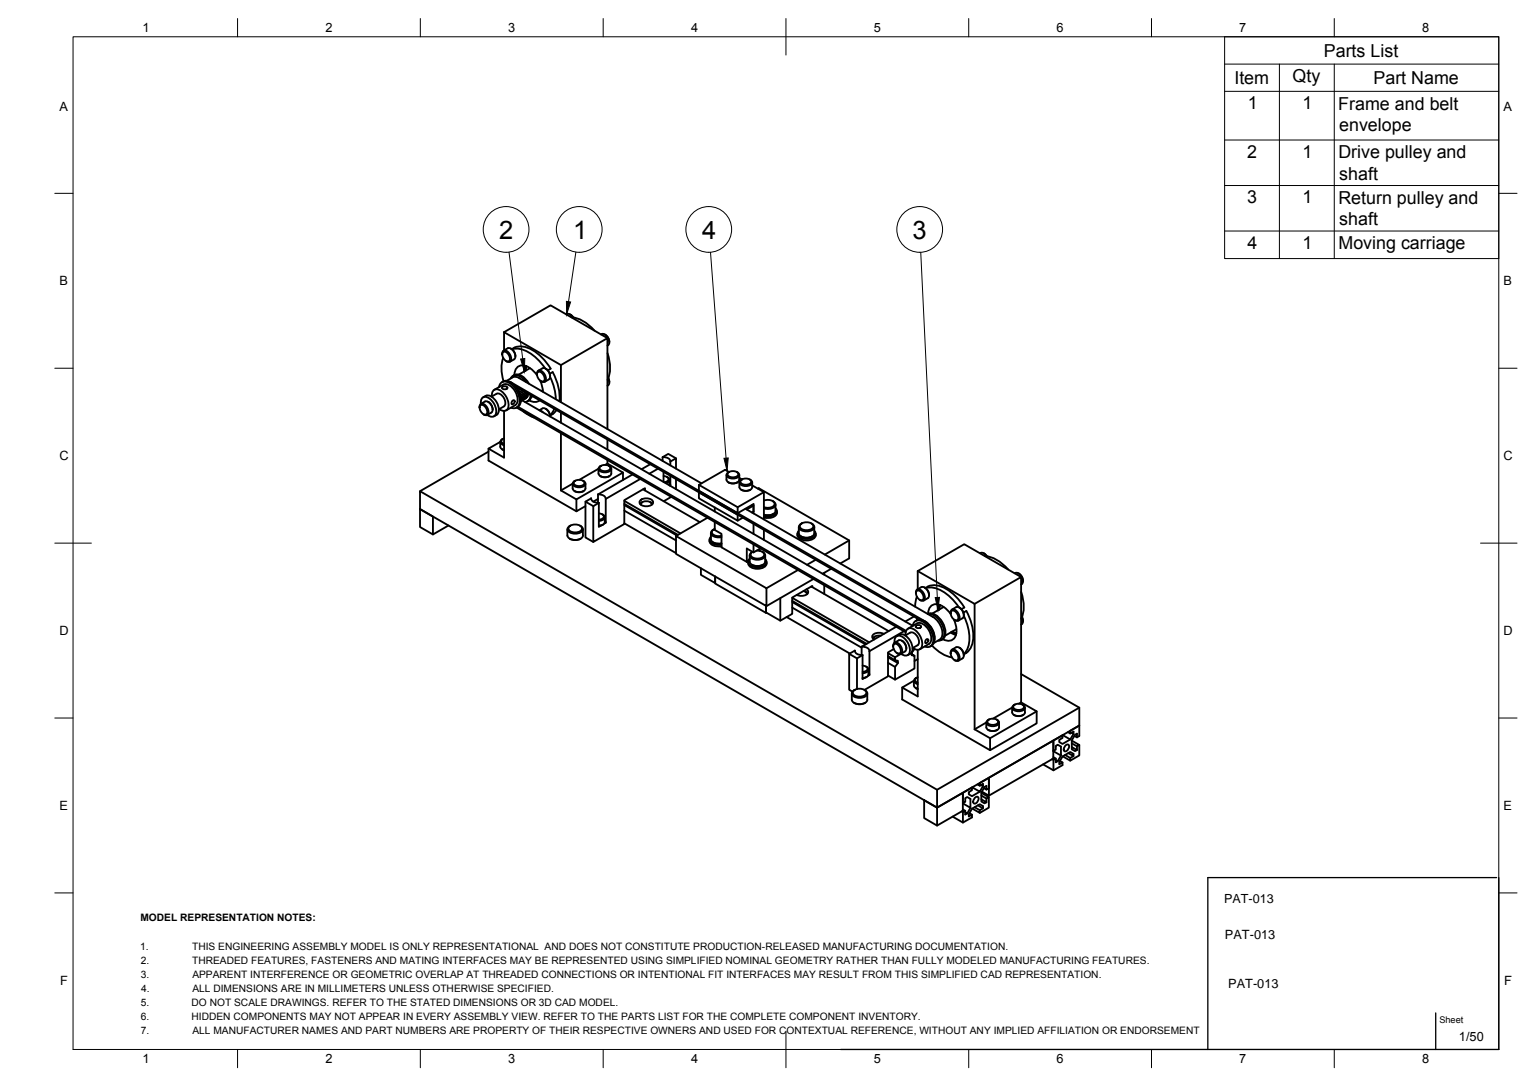
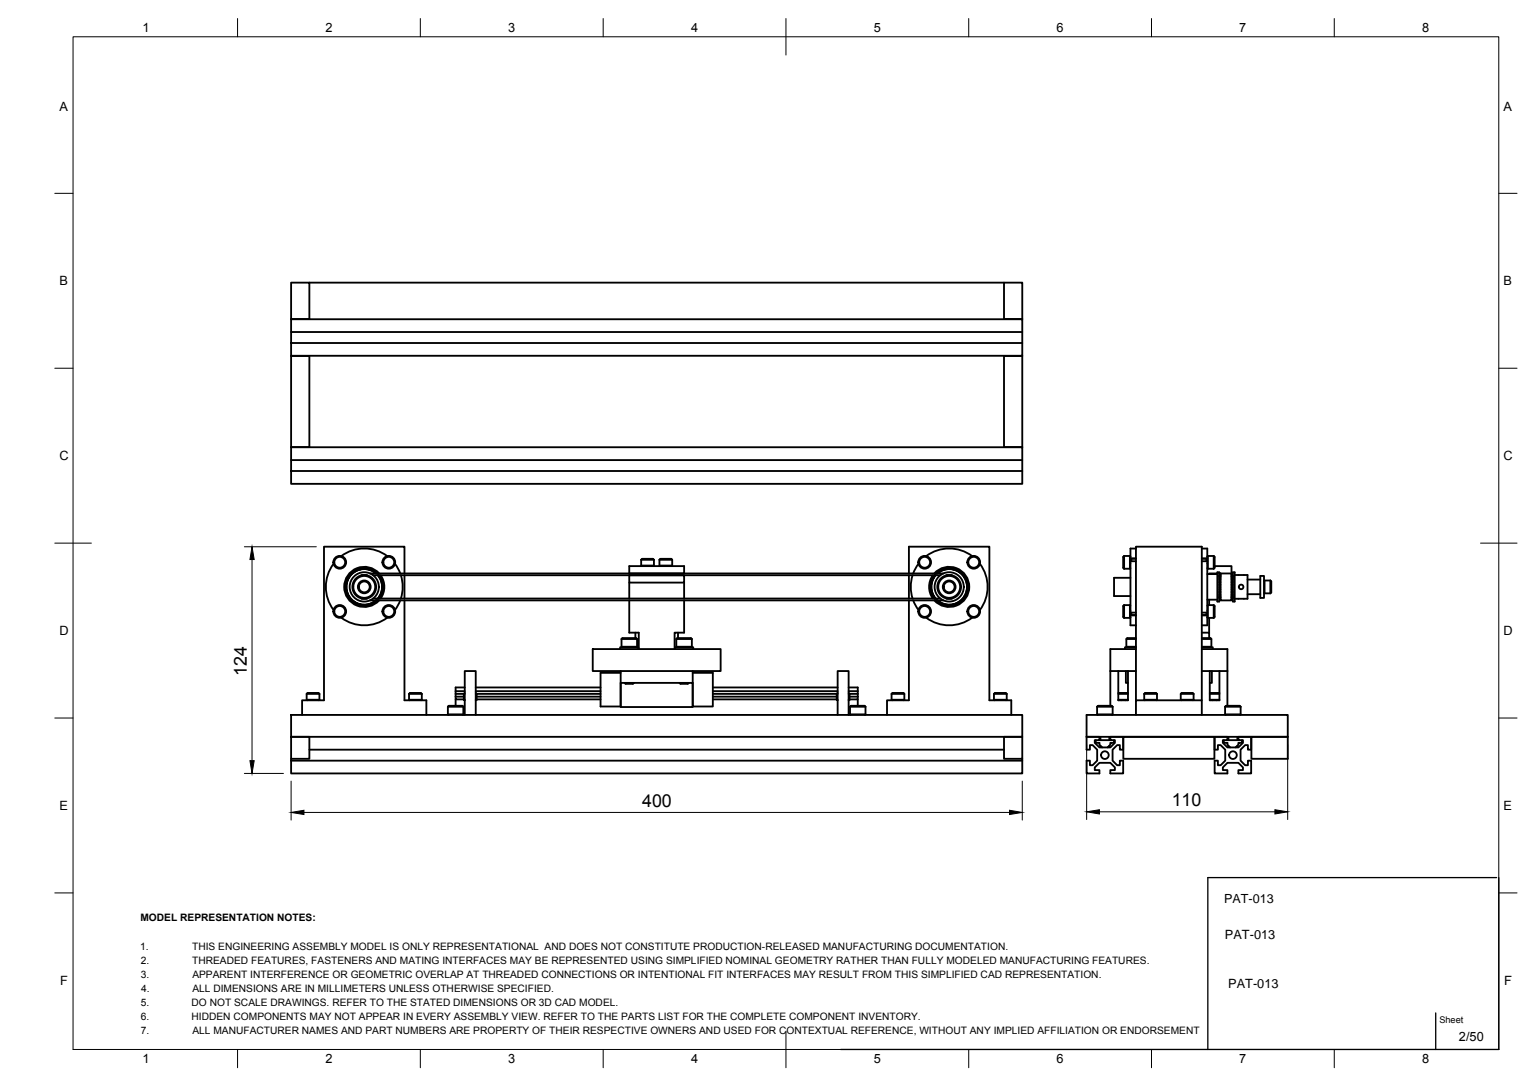
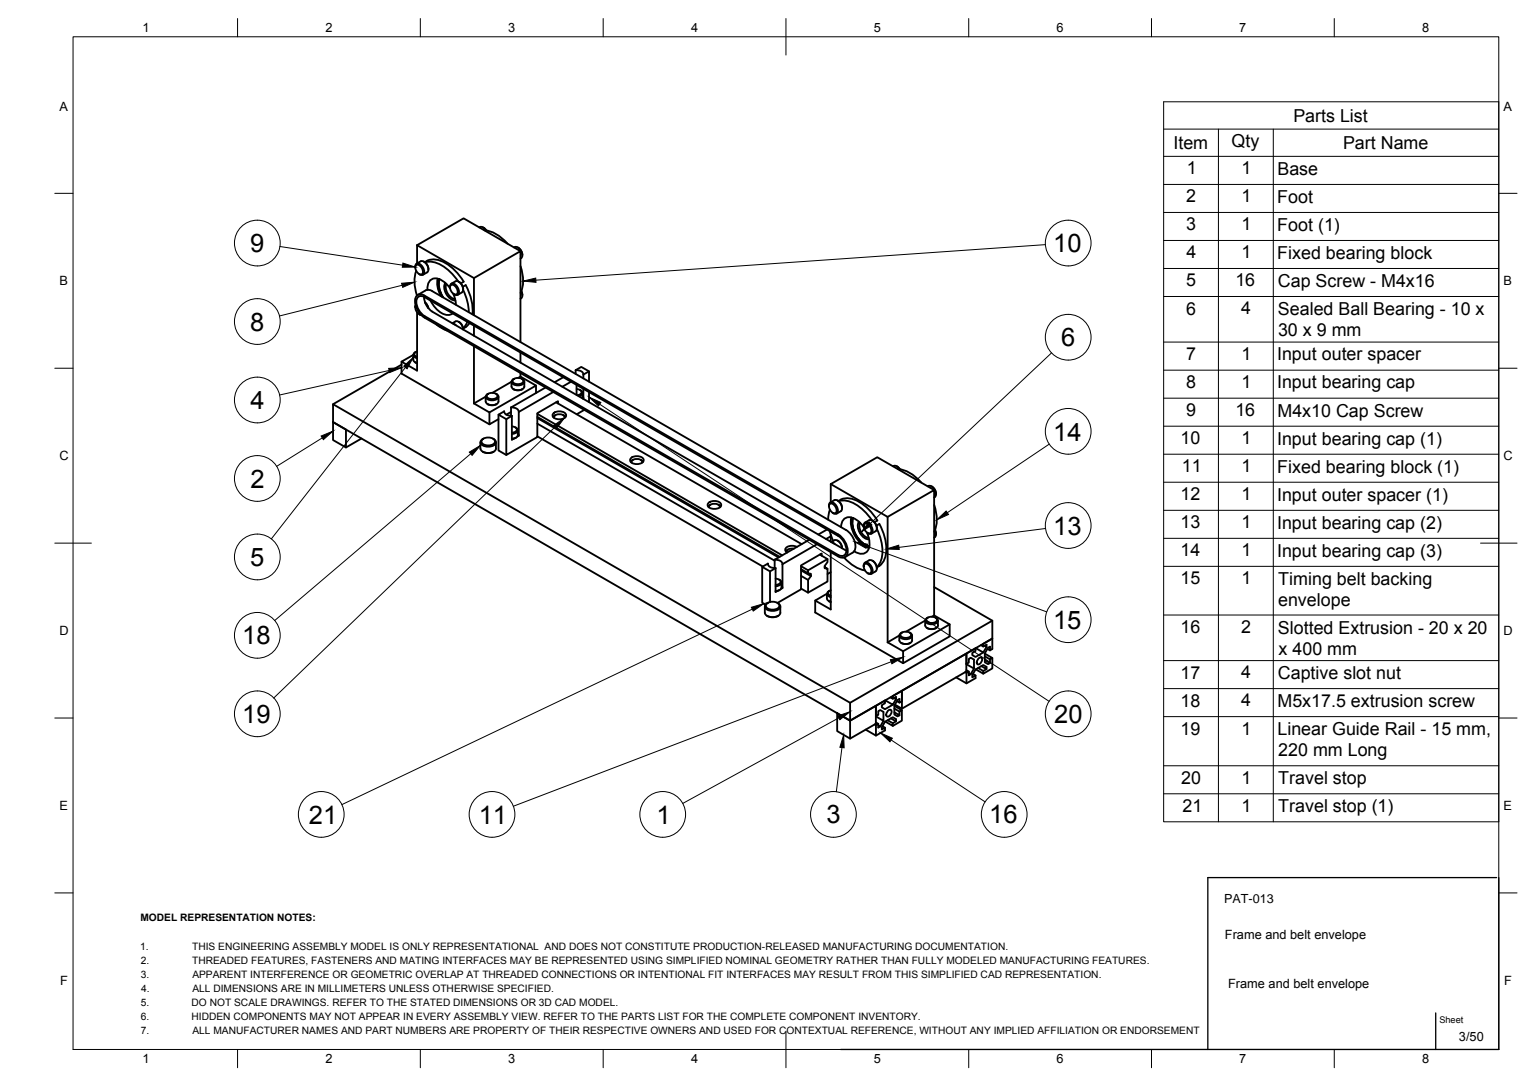
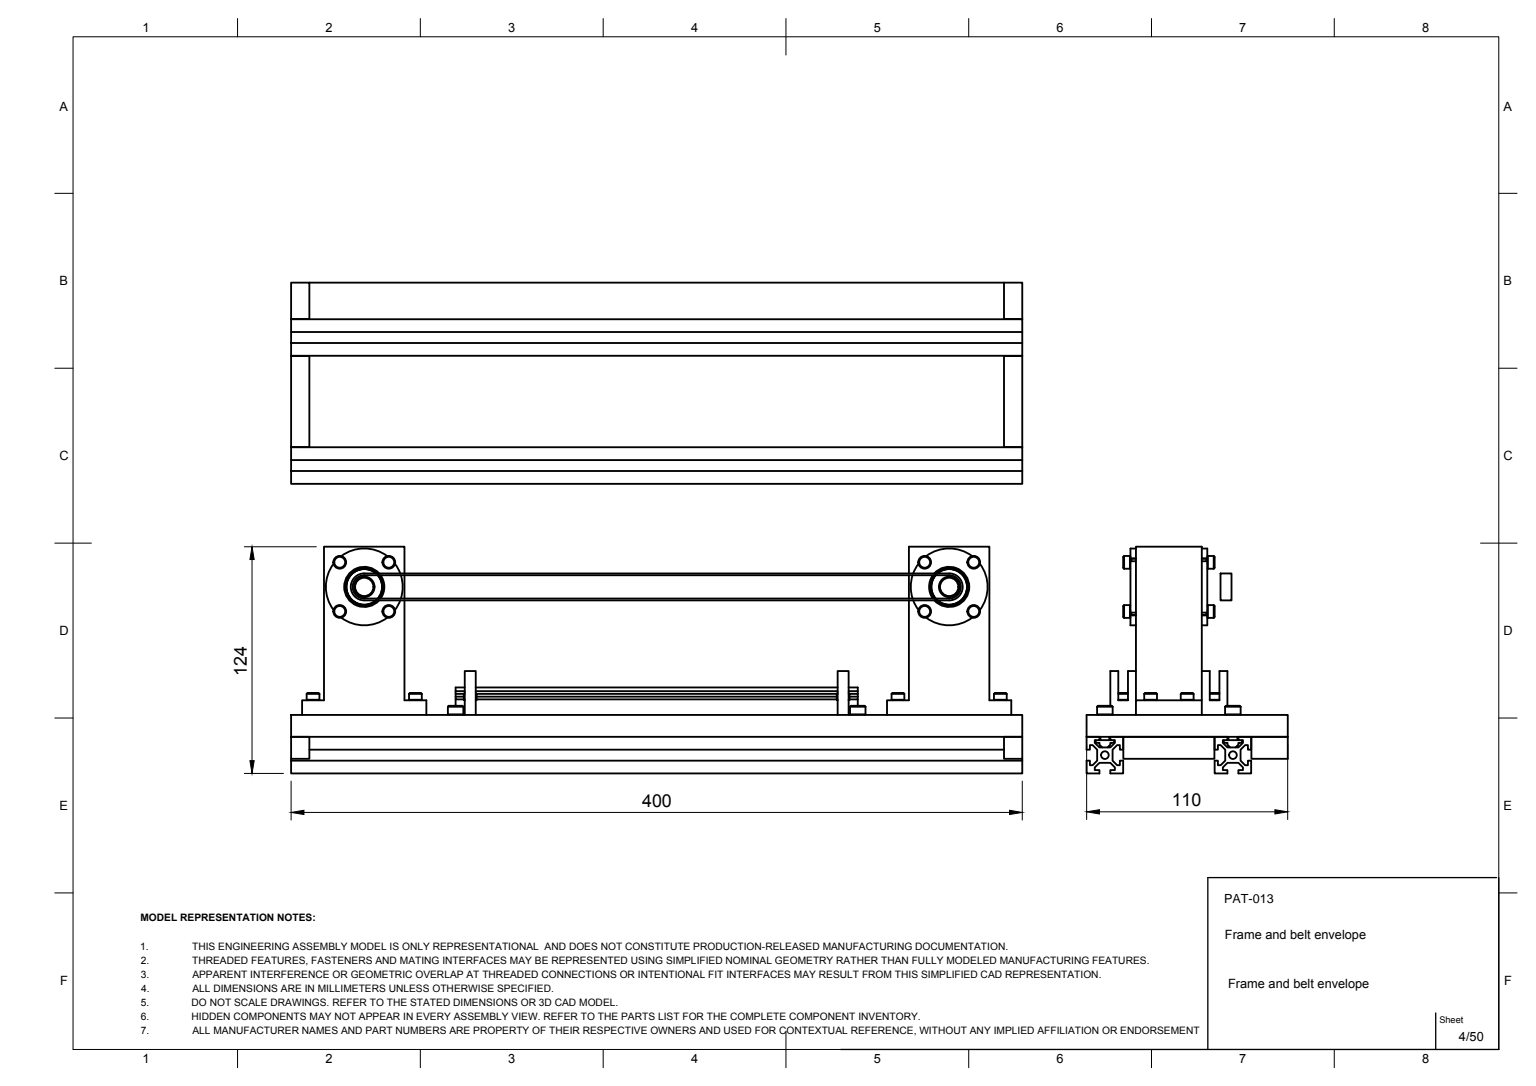
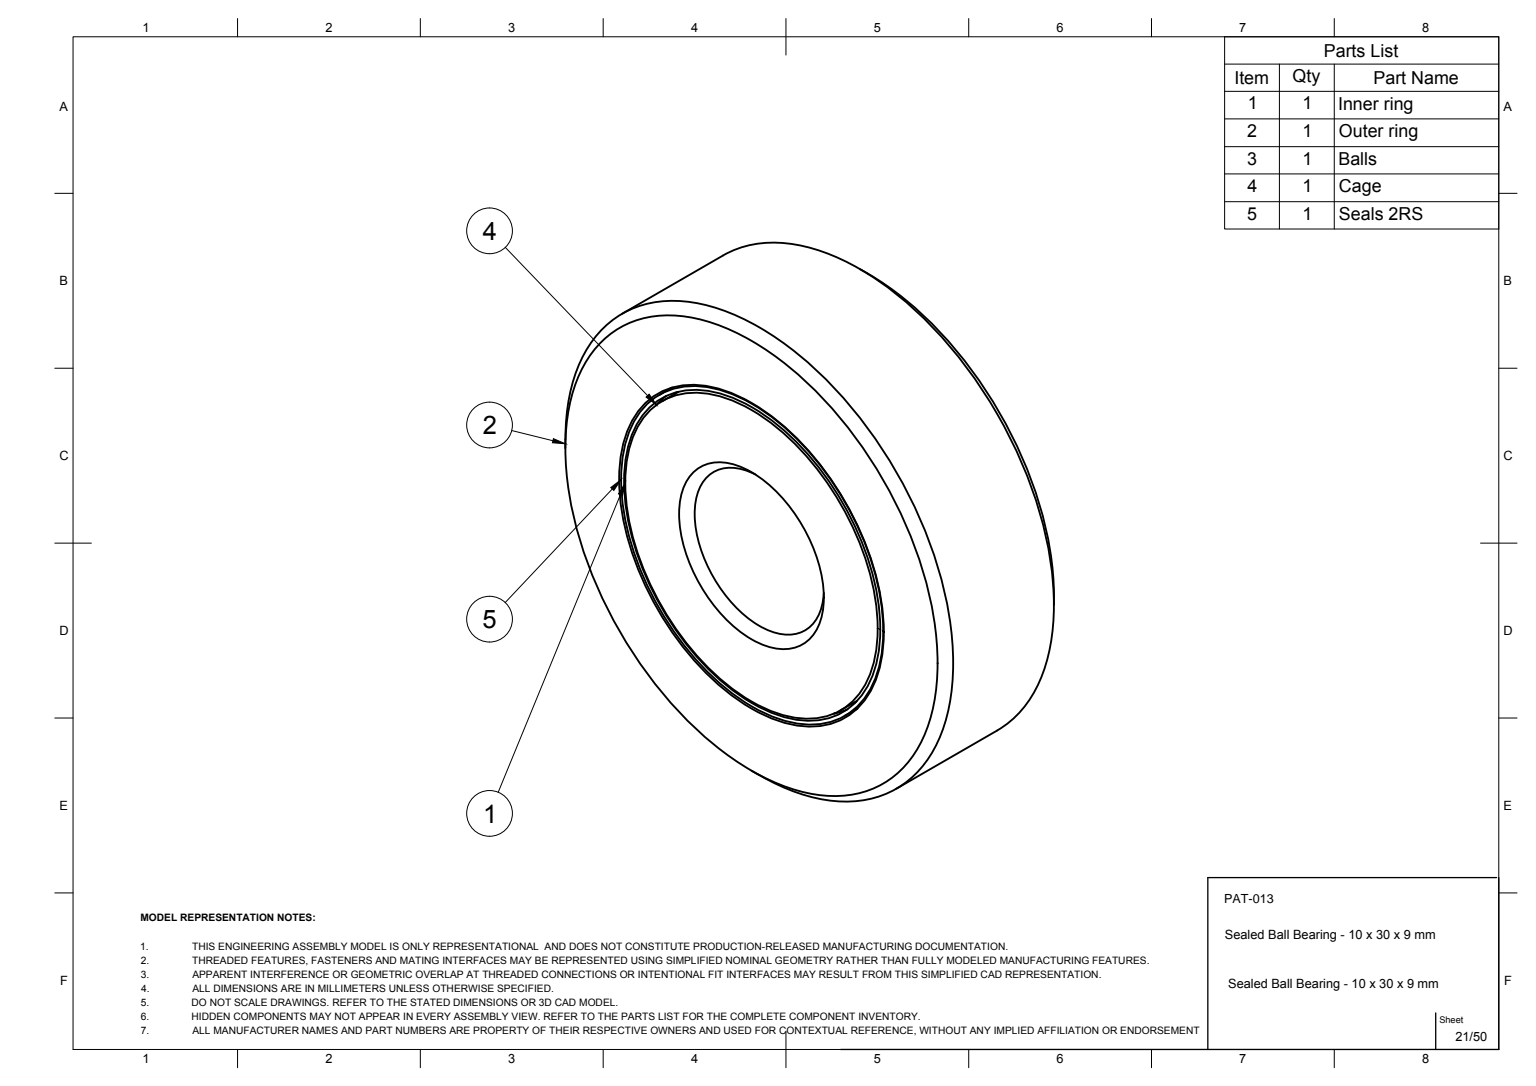
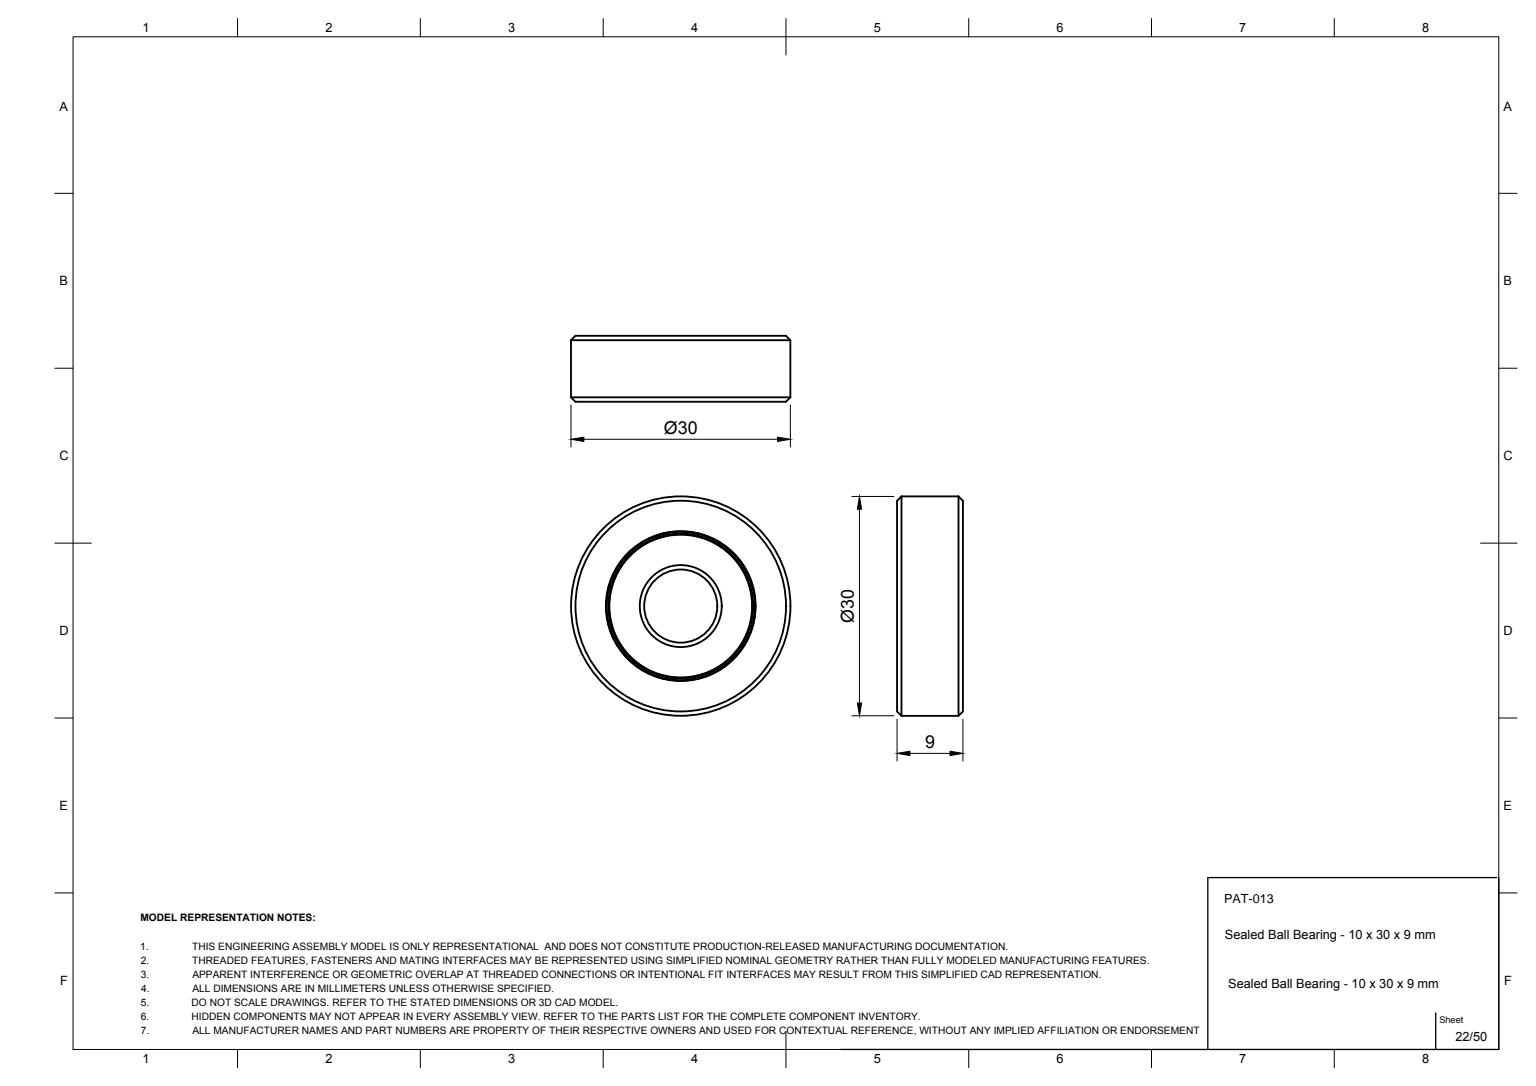
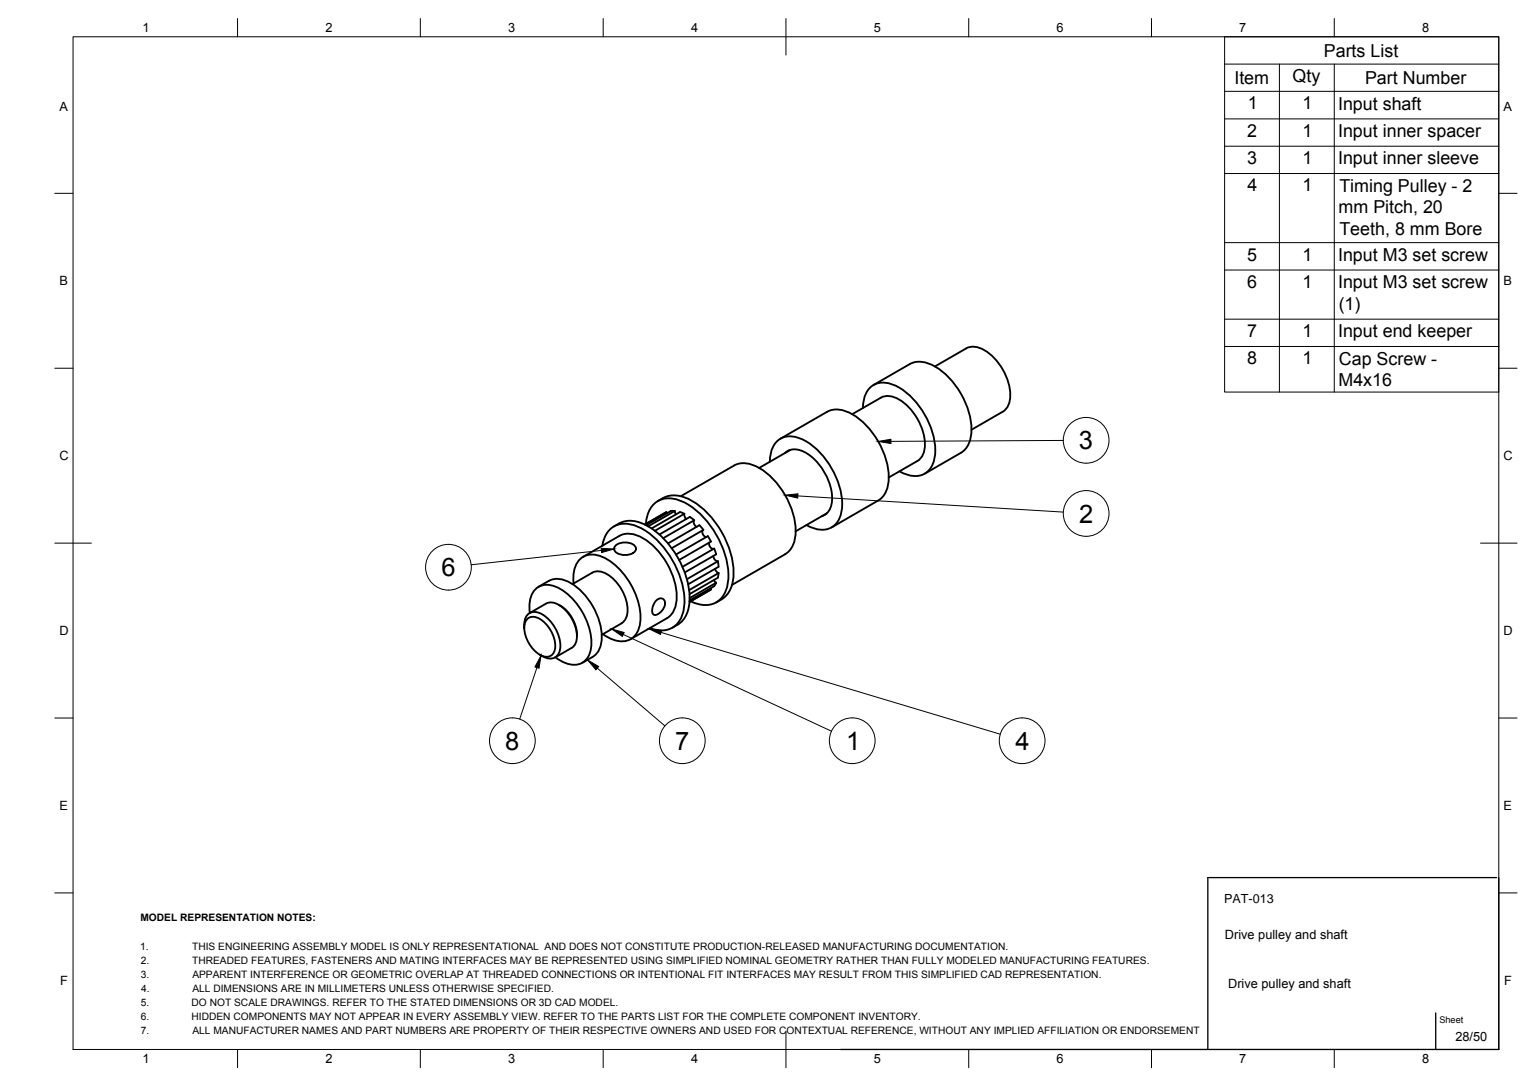
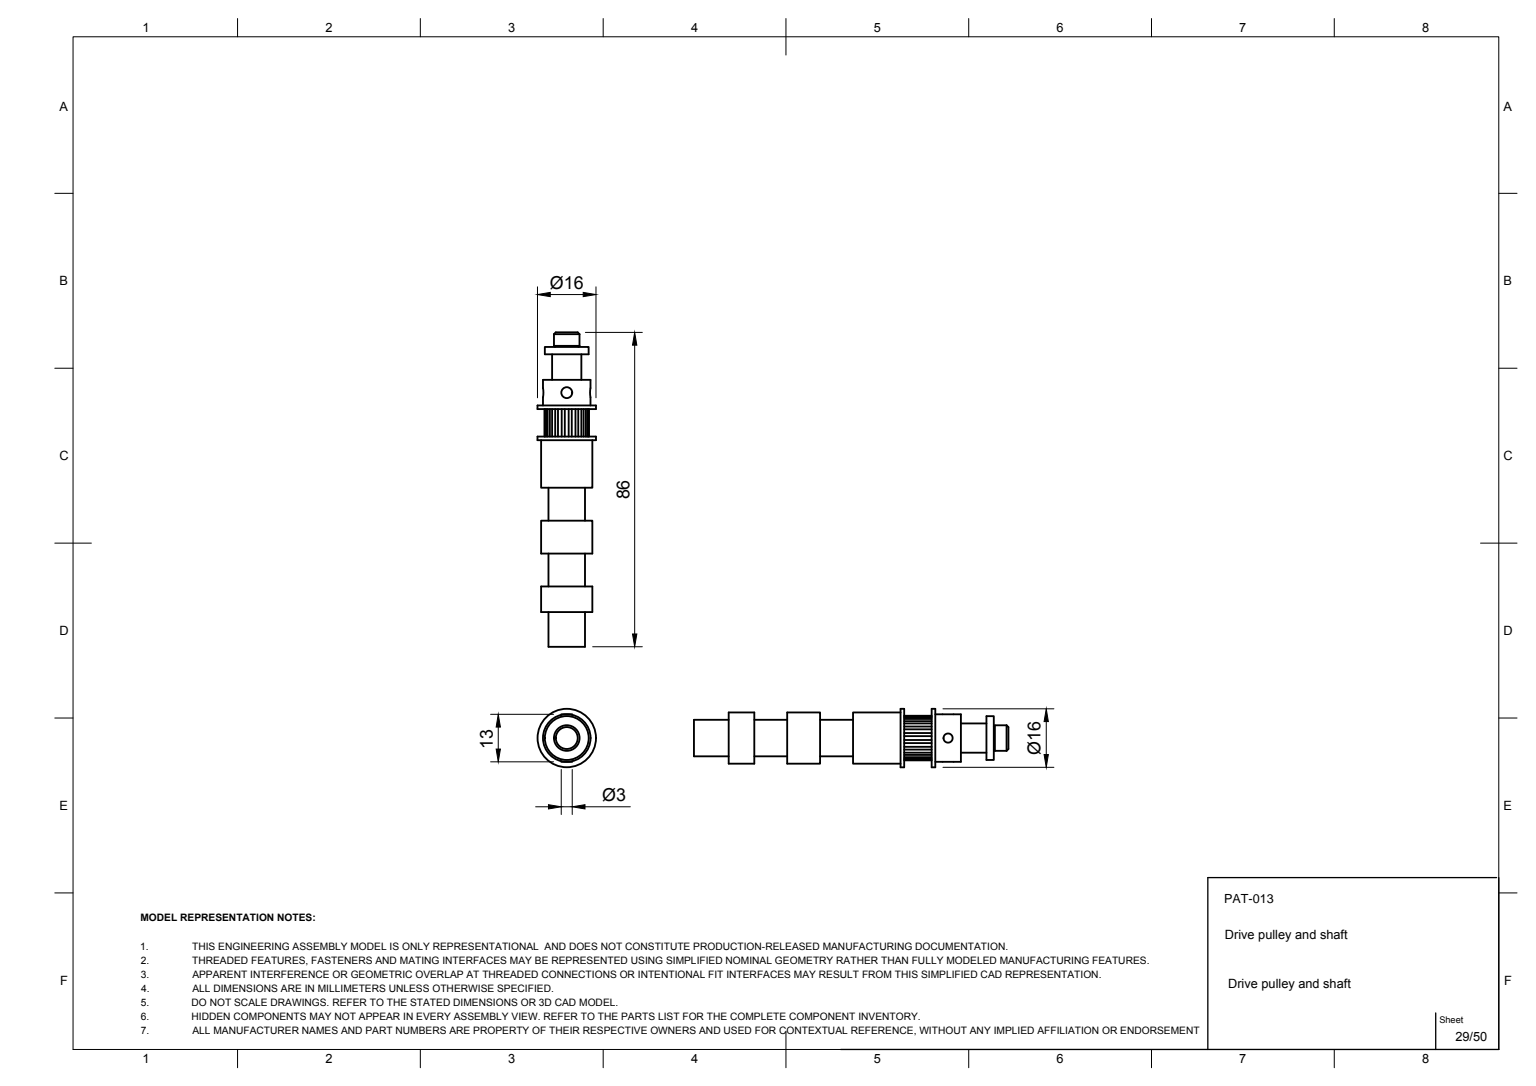
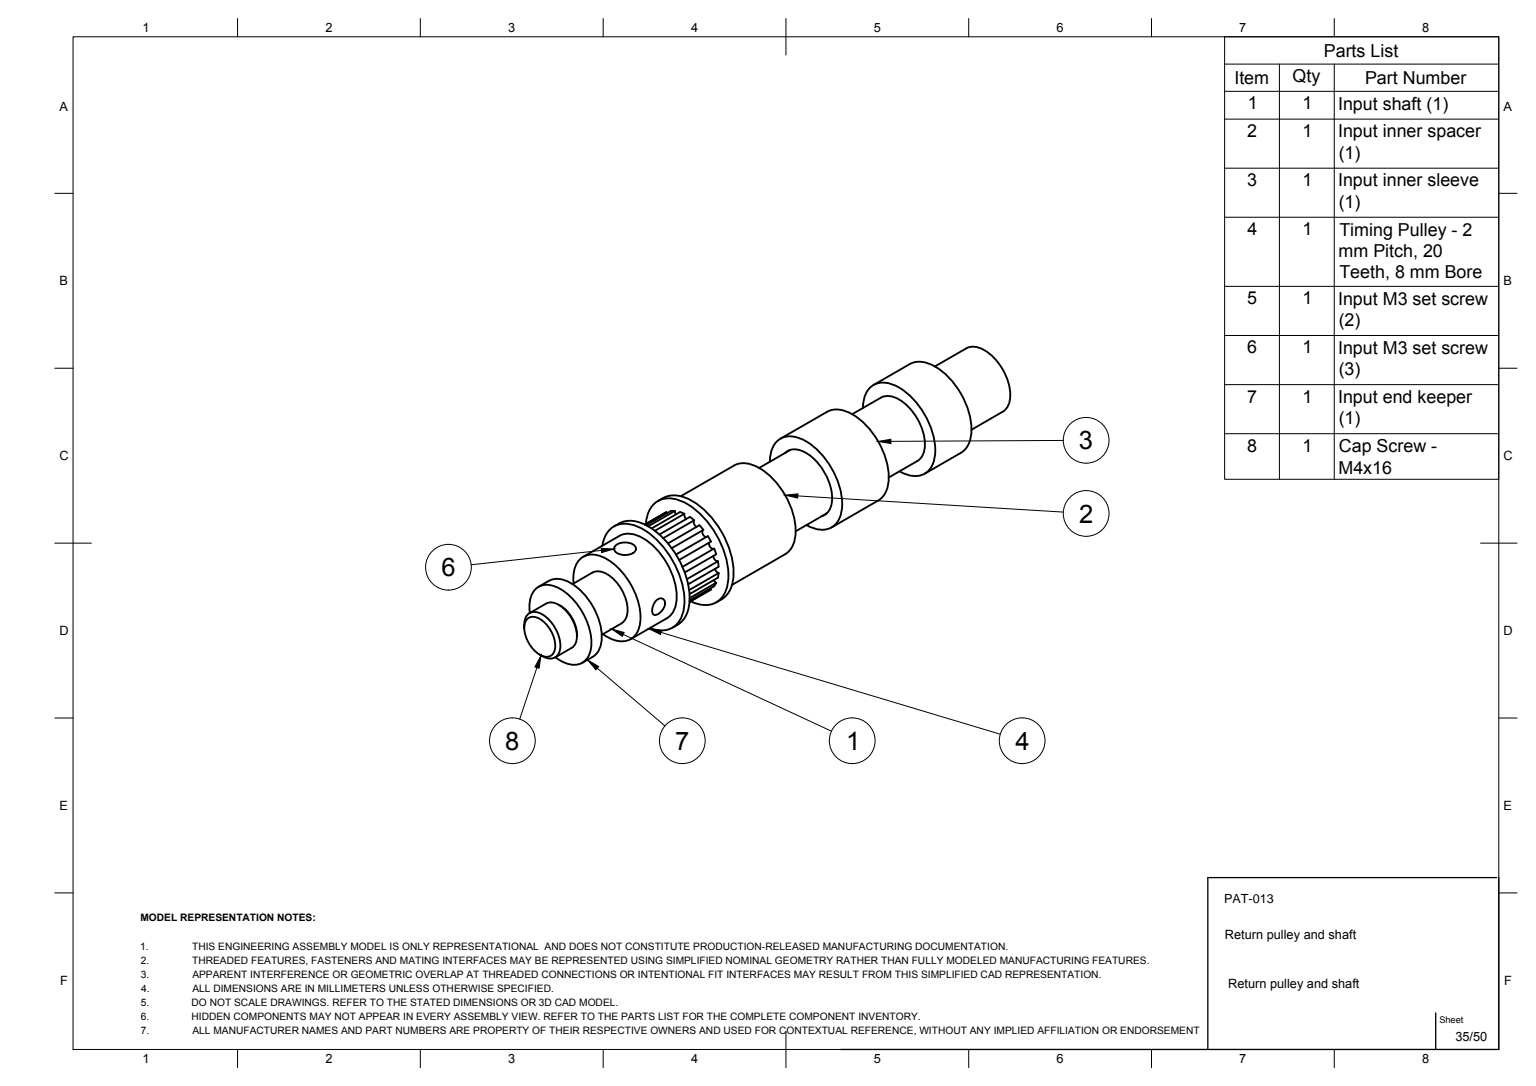
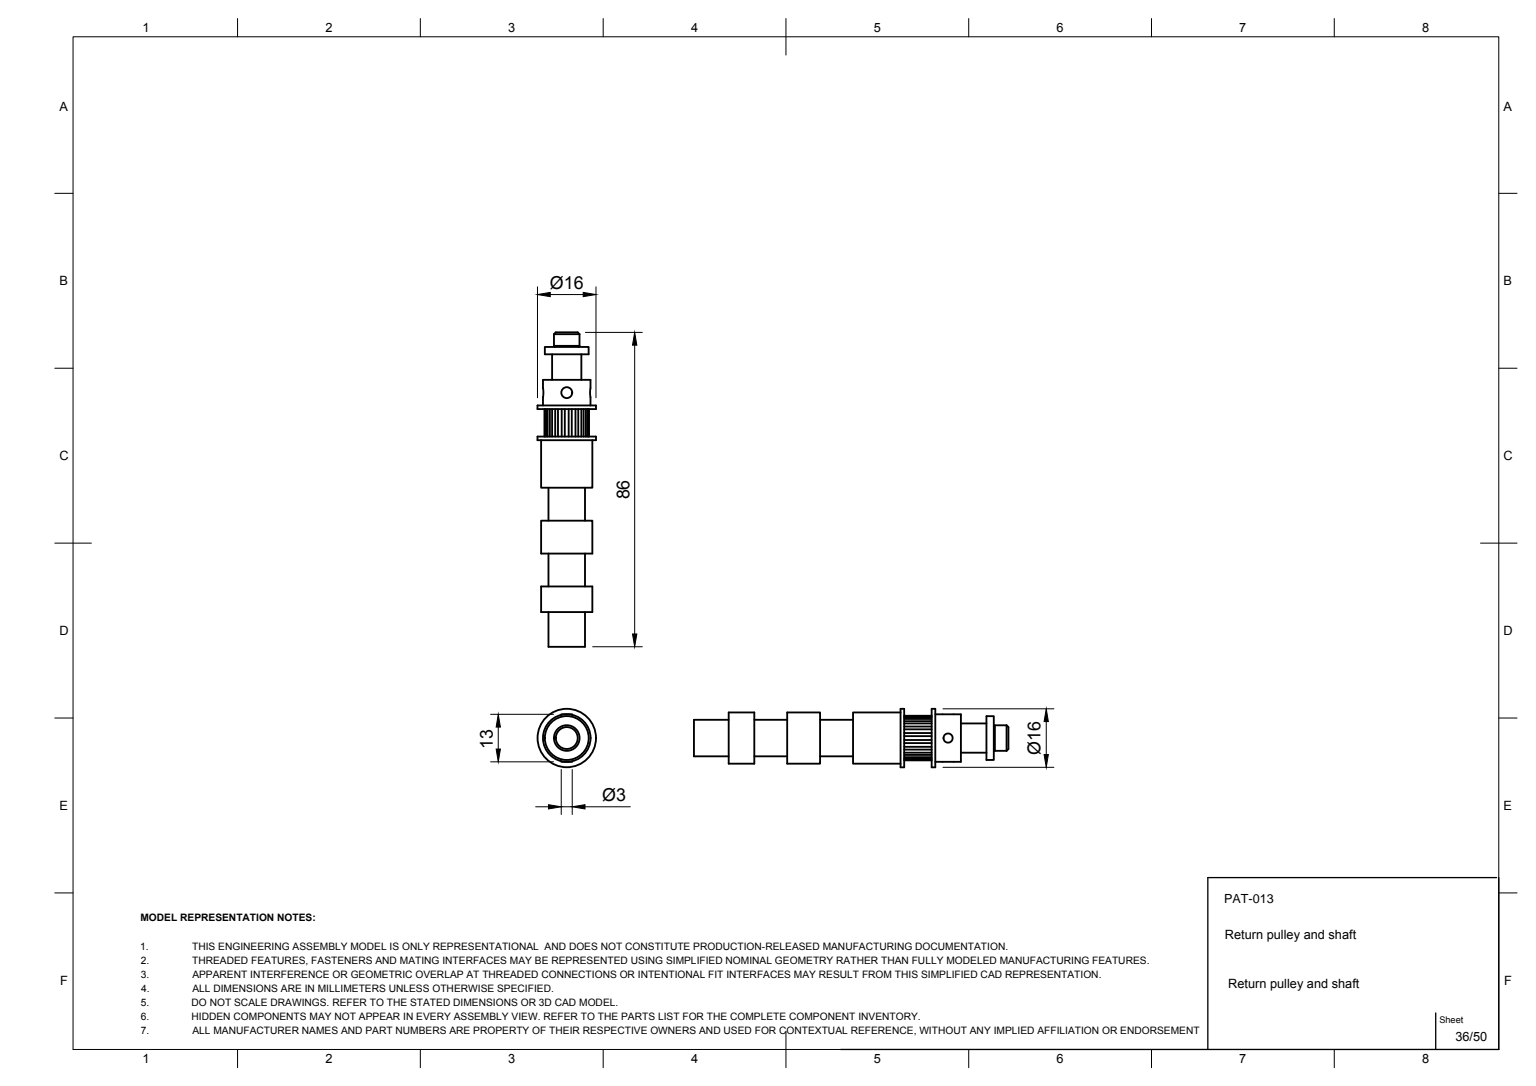
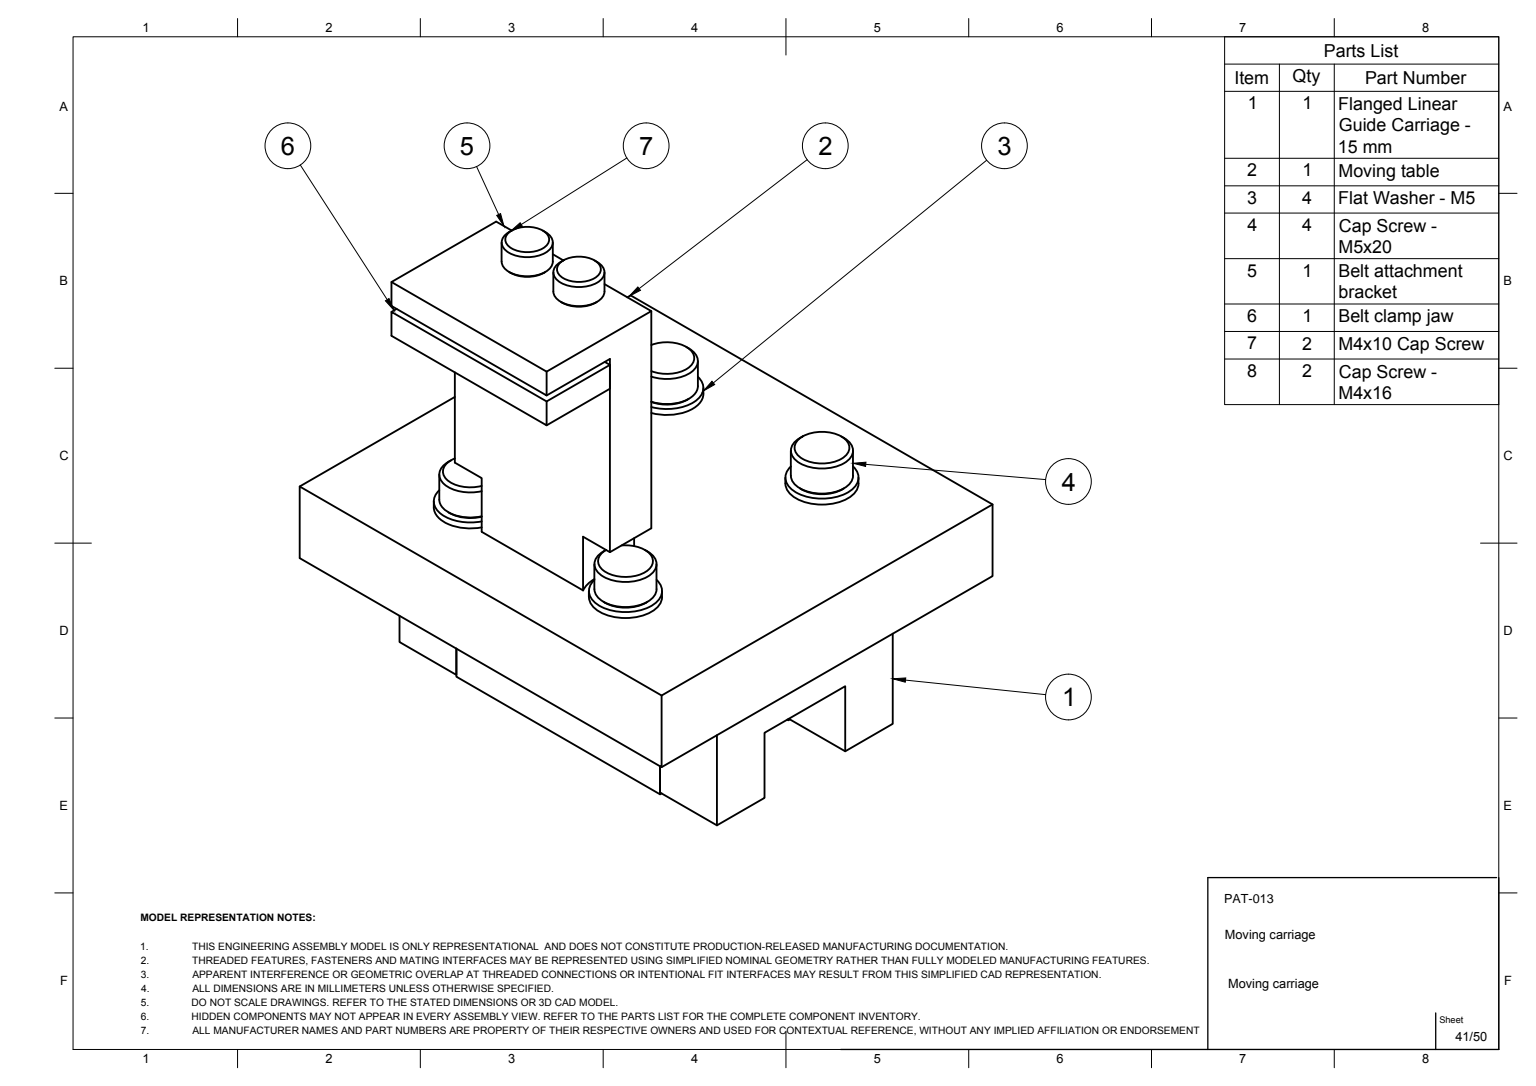
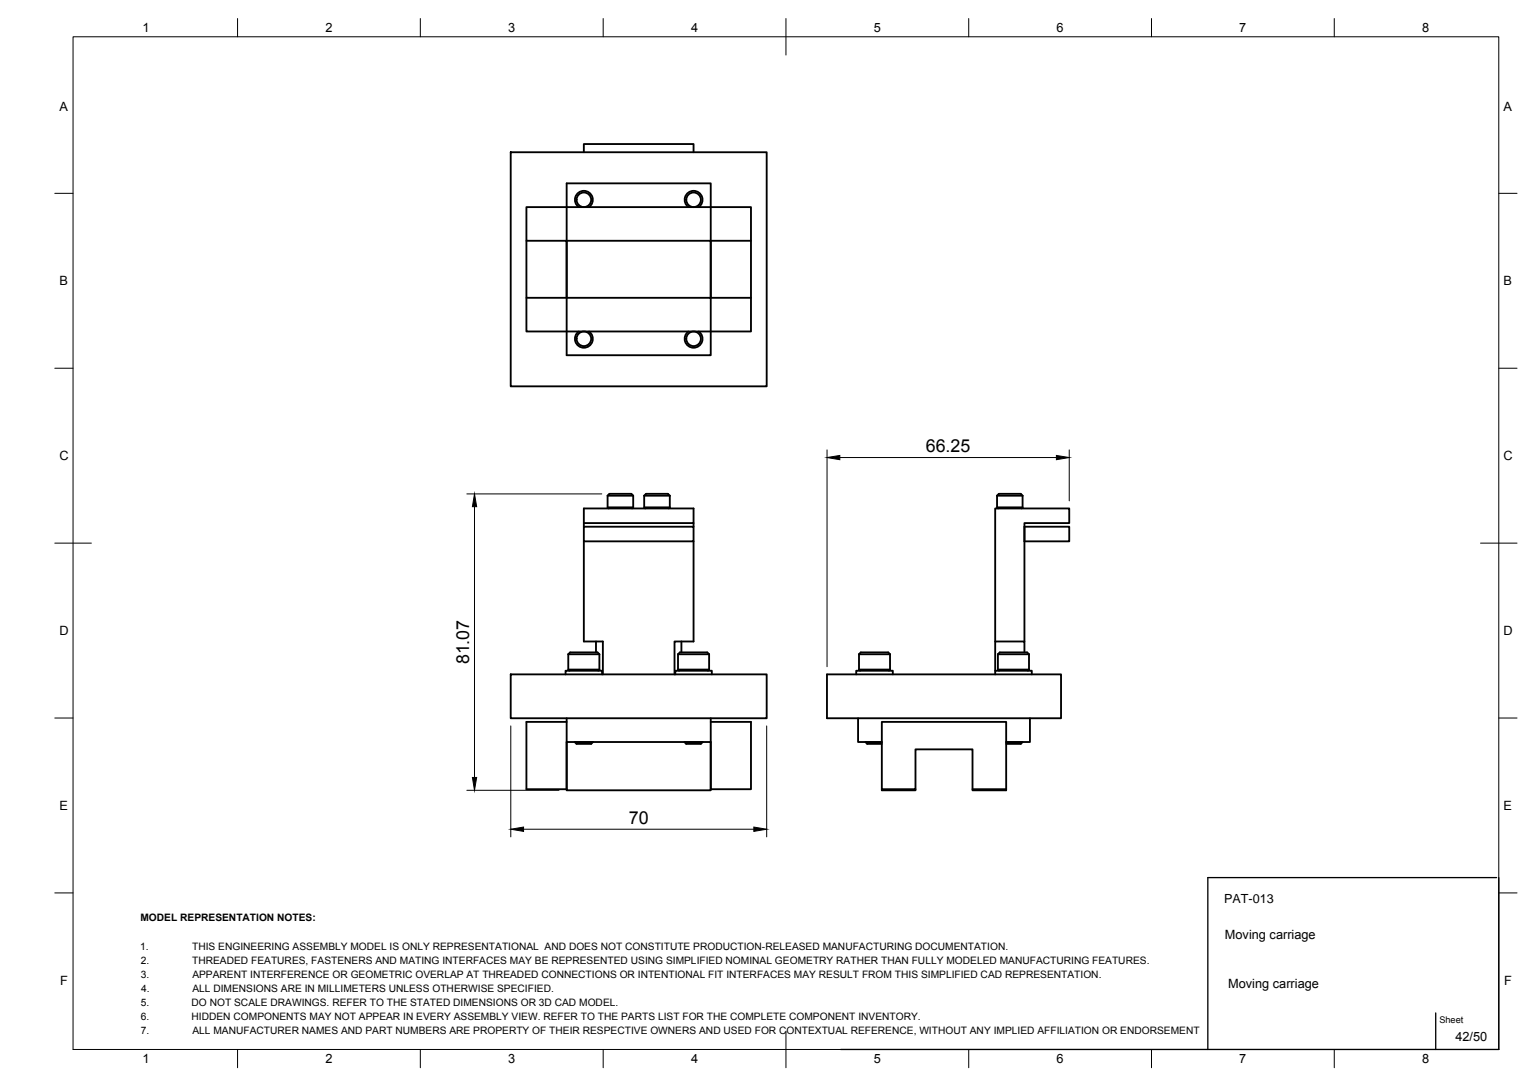
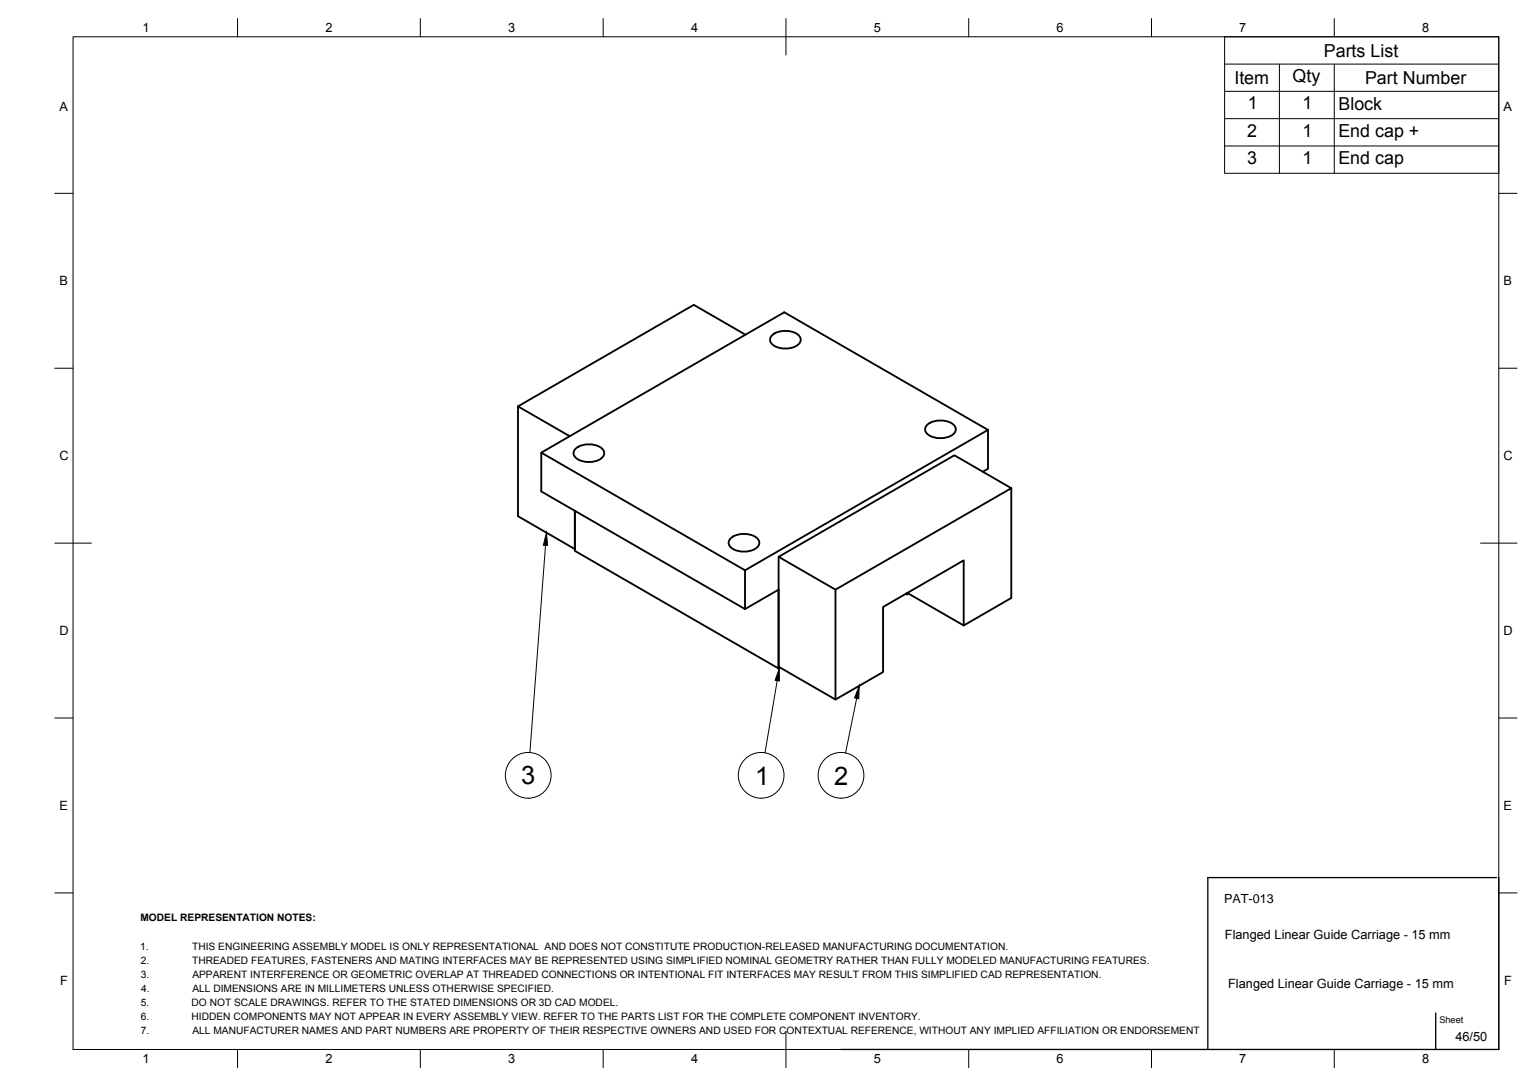
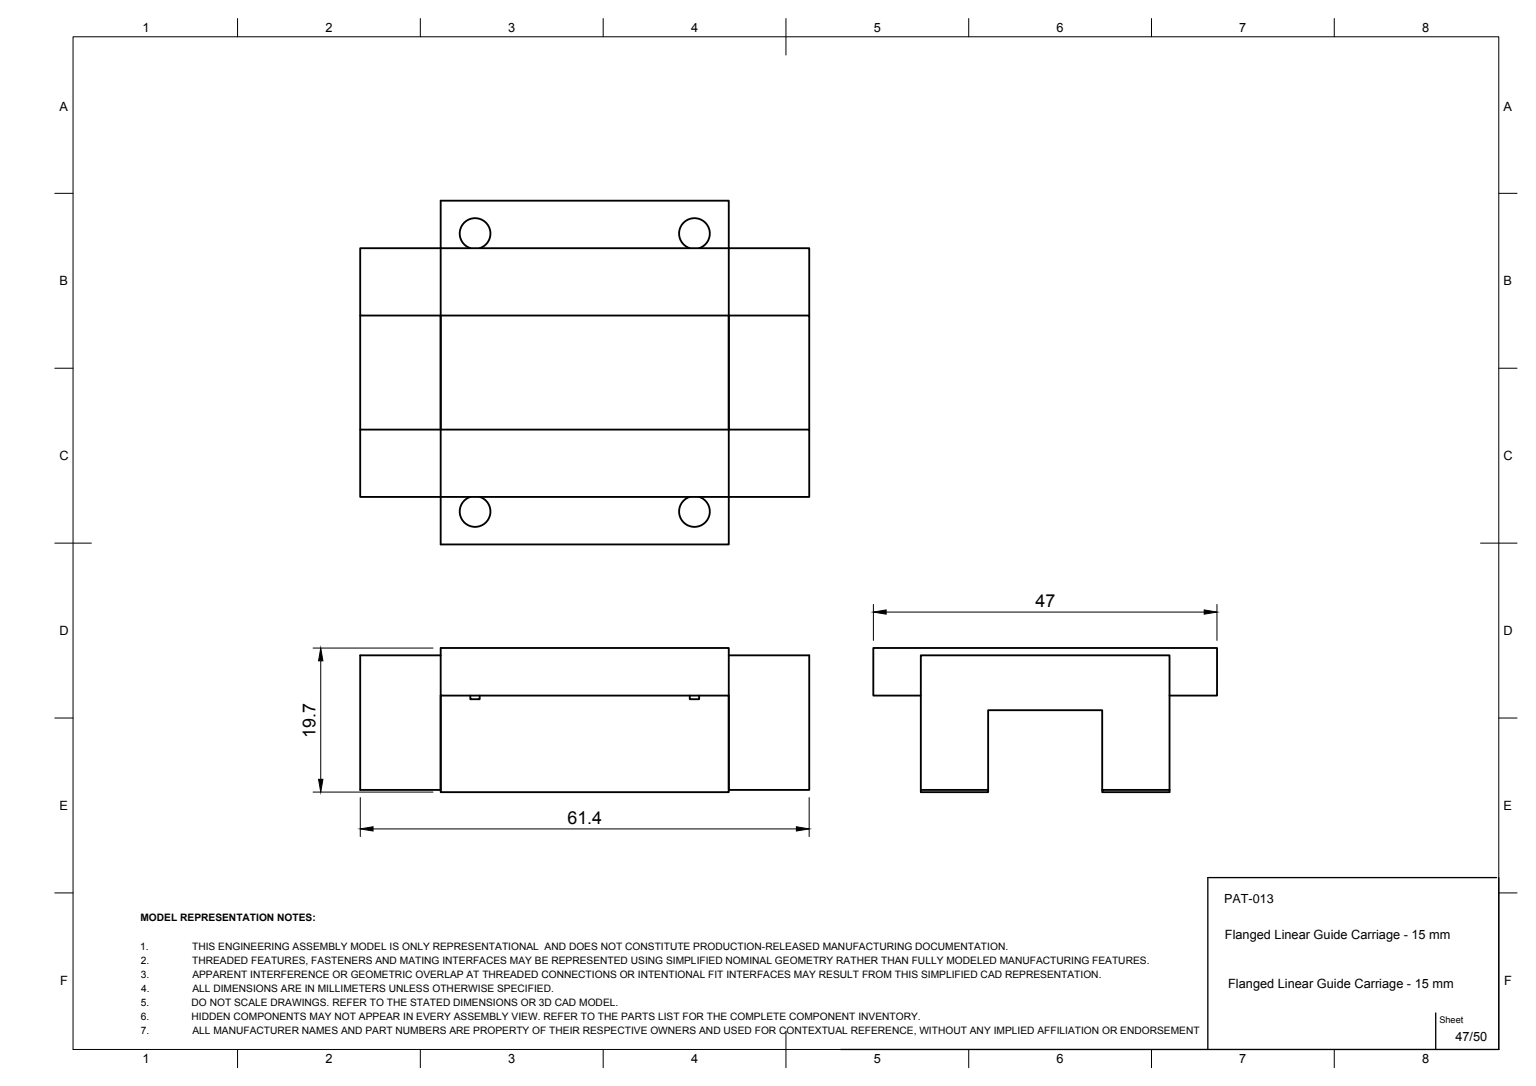
ISO-10303-21;
HEADER;
/* Generated by software containing ST-Developer
 * from STEP Tools, Inc. (www.steptools.com) 
 */

FILE_DESCRIPTION(
/* description */ ('Belt-driven linear axis on 2020 extrusion'),
/* implementation_level */ '2;1');

FILE_NAME(
/* name */ 'PAT-013',
/* time_stamp */ '2026-10-28T03:26:09-07:00',
/* author */ (''),
/* organization */ (''),
/* preprocessor_version */ 'ST-DEVELOPER v20.2',
/* originating_system */ 'Autodesk Translation Framework v15.17.0.0',
/* authorisation */ '');

FILE_SCHEMA (('AUTOMOTIVE_DESIGN { 1 0 10303 214 3 1 1 }'));
ENDSEC;

DATA;
#10=MECHANICAL_DESIGN_GEOMETRIC_PRESENTATION_REPRESENTATION('',(#610,#611,
#612,#613,#614,#615,#616,#617,#618,#619,#620,#621,#622,#623,#624,#625,#626,
#627,#628,#629,#630,#631,#632,#633,#634,#635,#636,#637,#638,#639,#640,#641,
#642,#643,#644,#645,#646,#647,#648,#649,#650,#651,#652,#653,#654,#655,#656,
#657,#658,#659,#660,#661,#662,#663,#664,#665),#20096);
#11=ORIENTED_CLOSED_SHELL('',*,#10954,.F.);
#12=ORIENTED_CLOSED_SHELL('',*,#10978,.F.);
#13=ORIENTED_CLOSED_SHELL('',*,#10979,.F.);
#14=ORIENTED_CLOSED_SHELL('',*,#10982,.F.);
#15=BREP_WITH_VOIDS('Body1',#10955,(#11));
#16=BREP_WITH_VOIDS('Body1',#10977,(#12));
#17=BREP_WITH_VOIDS('Body1',#10980,(#13));
#18=BREP_WITH_VOIDS('Body1',#10981,(#14));
#19=ELLIPSE('',#12111,0.299389011154384,0.2117);
#20=ELLIPSE('',#12115,0.299389011154384,0.2117);
#21=ITEM_DEFINED_TRANSFORMATION($,$,#11917,#12045);
#22=ITEM_DEFINED_TRANSFORMATION($,$,#11937,#12046);
#23=ITEM_DEFINED_TRANSFORMATION($,$,#11957,#12047);
#24=ITEM_DEFINED_TRANSFORMATION($,$,#11974,#12048);
#25=ITEM_DEFINED_TRANSFORMATION($,$,#12028,#12049);
#26=ITEM_DEFINED_TRANSFORMATION($,$,#12537,#12598);
#27=ITEM_DEFINED_TRANSFORMATION($,$,#12576,#12599);
#28=ITEM_DEFINED_TRANSFORMATION($,$,#12587,#12600);
#29=ITEM_DEFINED_TRANSFORMATION($,$,#11492,#12688);
#30=ITEM_DEFINED_TRANSFORMATION($,$,#11575,#12689);
#31=ITEM_DEFINED_TRANSFORMATION($,$,#11588,#12690);
#32=ITEM_DEFINED_TRANSFORMATION($,$,#11601,#12691);
#33=ITEM_DEFINED_TRANSFORMATION($,$,#11639,#12692);
#34=ITEM_DEFINED_TRANSFORMATION($,$,#11648,#12693);
#35=ITEM_DEFINED_TRANSFORMATION($,$,#11682,#12694);
#36=ITEM_DEFINED_TRANSFORMATION($,$,#11716,#12695);
#37=ITEM_DEFINED_TRANSFORMATION($,$,#11754,#12696);
#38=ITEM_DEFINED_TRANSFORMATION($,$,#11763,#12697);
#39=ITEM_DEFINED_TRANSFORMATION($,$,#11797,#12698);
#40=ITEM_DEFINED_TRANSFORMATION($,$,#11831,#12699);
#41=ITEM_DEFINED_TRANSFORMATION($,$,#11850,#12700);
#42=ITEM_DEFINED_TRANSFORMATION($,$,#11883,#12701);
#43=ITEM_DEFINED_TRANSFORMATION($,$,#12662,#12702);
#44=ITEM_DEFINED_TRANSFORMATION($,$,#12662,#12703);
#45=ITEM_DEFINED_TRANSFORMATION($,$,#12662,#12704);
#46=ITEM_DEFINED_TRANSFORMATION($,$,#12662,#12705);
#47=ITEM_DEFINED_TRANSFORMATION($,$,#11916,#12706);
#48=ITEM_DEFINED_TRANSFORMATION($,$,#11916,#12707);
#49=ITEM_DEFINED_TRANSFORMATION($,$,#12638,#12708);
#50=ITEM_DEFINED_TRANSFORMATION($,$,#12638,#12709);
#51=ITEM_DEFINED_TRANSFORMATION($,$,#12638,#12710);
#52=ITEM_DEFINED_TRANSFORMATION($,$,#12638,#12711);
#53=ITEM_DEFINED_TRANSFORMATION($,$,#12638,#12712);
#54=ITEM_DEFINED_TRANSFORMATION($,$,#12638,#12713);
#55=ITEM_DEFINED_TRANSFORMATION($,$,#12638,#12714);
#56=ITEM_DEFINED_TRANSFORMATION($,$,#12638,#12715);
#57=ITEM_DEFINED_TRANSFORMATION($,$,#12662,#12716);
#58=ITEM_DEFINED_TRANSFORMATION($,$,#12662,#12717);
#59=ITEM_DEFINED_TRANSFORMATION($,$,#12662,#12718);
#60=ITEM_DEFINED_TRANSFORMATION($,$,#12662,#12719);
#61=ITEM_DEFINED_TRANSFORMATION($,$,#11916,#12720);
#62=ITEM_DEFINED_TRANSFORMATION($,$,#11916,#12721);
#63=ITEM_DEFINED_TRANSFORMATION($,$,#12638,#12722);
#64=ITEM_DEFINED_TRANSFORMATION($,$,#12638,#12723);
#65=ITEM_DEFINED_TRANSFORMATION($,$,#12638,#12724);
#66=ITEM_DEFINED_TRANSFORMATION($,$,#12638,#12725);
#67=ITEM_DEFINED_TRANSFORMATION($,$,#12638,#12726);
#68=ITEM_DEFINED_TRANSFORMATION($,$,#12638,#12727);
#69=ITEM_DEFINED_TRANSFORMATION($,$,#12638,#12728);
#70=ITEM_DEFINED_TRANSFORMATION($,$,#12638,#12729);
#71=ITEM_DEFINED_TRANSFORMATION($,$,#12050,#12730);
#72=ITEM_DEFINED_TRANSFORMATION($,$,#12100,#12731);
#73=ITEM_DEFINED_TRANSFORMATION($,$,#12121,#12732);
#74=ITEM_DEFINED_TRANSFORMATION($,$,#12100,#12733);
#75=ITEM_DEFINED_TRANSFORMATION($,$,#12121,#12734);
#76=ITEM_DEFINED_TRANSFORMATION($,$,#12050,#12735);
#77=ITEM_DEFINED_TRANSFORMATION($,$,#12100,#12736);
#78=ITEM_DEFINED_TRANSFORMATION($,$,#12121,#12737);
#79=ITEM_DEFINED_TRANSFORMATION($,$,#12100,#12738);
#80=ITEM_DEFINED_TRANSFORMATION($,$,#12121,#12739);
#81=ITEM_DEFINED_TRANSFORMATION($,$,#12145,#12740);
#82=ITEM_DEFINED_TRANSFORMATION($,$,#12662,#12741);
#83=ITEM_DEFINED_TRANSFORMATION($,$,#12662,#12742);
#84=ITEM_DEFINED_TRANSFORMATION($,$,#12662,#12743);
#85=ITEM_DEFINED_TRANSFORMATION($,$,#12662,#12744);
#86=ITEM_DEFINED_TRANSFORMATION($,$,#12662,#12745);
#87=ITEM_DEFINED_TRANSFORMATION($,$,#12662,#12746);
#88=ITEM_DEFINED_TRANSFORMATION($,$,#12662,#12747);
#89=ITEM_DEFINED_TRANSFORMATION($,$,#12662,#12748);
#90=ITEM_DEFINED_TRANSFORMATION($,$,#12189,#12749);
#91=ITEM_DEFINED_TRANSFORMATION($,$,#12211,#12750);
#92=ITEM_DEFINED_TRANSFORMATION($,$,#12224,#12751);
#93=ITEM_DEFINED_TRANSFORMATION($,$,#12233,#12752);
#94=ITEM_DEFINED_TRANSFORMATION($,$,#12239,#12753);
#95=ITEM_DEFINED_TRANSFORMATION($,$,#12245,#12754);
#96=ITEM_DEFINED_TRANSFORMATION($,$,#12320,#12755);
#97=ITEM_DEFINED_TRANSFORMATION($,$,#12662,#12756);
#98=ITEM_DEFINED_TRANSFORMATION($,$,#12255,#12757);
#99=ITEM_DEFINED_TRANSFORMATION($,$,#12277,#12758);
#100=ITEM_DEFINED_TRANSFORMATION($,$,#12290,#12759);
#101=ITEM_DEFINED_TRANSFORMATION($,$,#12299,#12760);
#102=ITEM_DEFINED_TRANSFORMATION($,$,#12305,#12761);
#103=ITEM_DEFINED_TRANSFORMATION($,$,#12311,#12762);
#104=ITEM_DEFINED_TRANSFORMATION($,$,#12320,#12763);
#105=ITEM_DEFINED_TRANSFORMATION($,$,#12662,#12764);
#106=ITEM_DEFINED_TRANSFORMATION($,$,#12463,#12765);
#107=ITEM_DEFINED_TRANSFORMATION($,$,#12496,#12766);
#108=ITEM_DEFINED_TRANSFORMATION($,$,#12529,#12767);
#109=ITEM_DEFINED_TRANSFORMATION($,$,#12536,#12768);
#110=ITEM_DEFINED_TRANSFORMATION($,$,#12601,#12769);
#111=ITEM_DEFINED_TRANSFORMATION($,$,#12612,#12770);
#112=ITEM_DEFINED_TRANSFORMATION($,$,#12601,#12771);
#113=ITEM_DEFINED_TRANSFORMATION($,$,#12612,#12772);
#114=ITEM_DEFINED_TRANSFORMATION($,$,#12601,#12773);
#115=ITEM_DEFINED_TRANSFORMATION($,$,#12612,#12774);
#116=ITEM_DEFINED_TRANSFORMATION($,$,#12601,#12775);
#117=ITEM_DEFINED_TRANSFORMATION($,$,#12612,#12776);
#118=ITEM_DEFINED_TRANSFORMATION($,$,#12638,#12777);
#119=ITEM_DEFINED_TRANSFORMATION($,$,#12638,#12778);
#120=ITEM_DEFINED_TRANSFORMATION($,$,#12662,#12779);
#121=ITEM_DEFINED_TRANSFORMATION($,$,#12662,#12780);
#122=ITEM_DEFINED_TRANSFORMATION($,$,#11491,#12781);
#123=ITEM_DEFINED_TRANSFORMATION($,$,#12188,#12782);
#124=ITEM_DEFINED_TRANSFORMATION($,$,#12254,#12783);
#125=ITEM_DEFINED_TRANSFORMATION($,$,#12462,#12784);
#126=(
REPRESENTATION_RELATIONSHIP($,$,#20329,#20328)
REPRESENTATION_RELATIONSHIP_WITH_TRANSFORMATION(#21)
SHAPE_REPRESENTATION_RELATIONSHIP()
);
#127=(
REPRESENTATION_RELATIONSHIP($,$,#20330,#20328)
REPRESENTATION_RELATIONSHIP_WITH_TRANSFORMATION(#22)
SHAPE_REPRESENTATION_RELATIONSHIP()
);
#128=(
REPRESENTATION_RELATIONSHIP($,$,#20331,#20328)
REPRESENTATION_RELATIONSHIP_WITH_TRANSFORMATION(#23)
SHAPE_REPRESENTATION_RELATIONSHIP()
);
#129=(
REPRESENTATION_RELATIONSHIP($,$,#20332,#20328)
REPRESENTATION_RELATIONSHIP_WITH_TRANSFORMATION(#24)
SHAPE_REPRESENTATION_RELATIONSHIP()
);
#130=(
REPRESENTATION_RELATIONSHIP($,$,#20333,#20328)
REPRESENTATION_RELATIONSHIP_WITH_TRANSFORMATION(#25)
SHAPE_REPRESENTATION_RELATIONSHIP()
);
#131=(
REPRESENTATION_RELATIONSHIP($,$,#20358,#20357)
REPRESENTATION_RELATIONSHIP_WITH_TRANSFORMATION(#26)
SHAPE_REPRESENTATION_RELATIONSHIP()
);
#132=(
REPRESENTATION_RELATIONSHIP($,$,#20359,#20357)
REPRESENTATION_RELATIONSHIP_WITH_TRANSFORMATION(#27)
SHAPE_REPRESENTATION_RELATIONSHIP()
);
#133=(
REPRESENTATION_RELATIONSHIP($,$,#20360,#20357)
REPRESENTATION_RELATIONSHIP_WITH_TRANSFORMATION(#28)
SHAPE_REPRESENTATION_RELATIONSHIP()
);
#134=(
REPRESENTATION_RELATIONSHIP($,$,#20314,#20313)
REPRESENTATION_RELATIONSHIP_WITH_TRANSFORMATION(#29)
SHAPE_REPRESENTATION_RELATIONSHIP()
);
#135=(
REPRESENTATION_RELATIONSHIP($,$,#20315,#20313)
REPRESENTATION_RELATIONSHIP_WITH_TRANSFORMATION(#30)
SHAPE_REPRESENTATION_RELATIONSHIP()
);
#136=(
REPRESENTATION_RELATIONSHIP($,$,#20316,#20313)
REPRESENTATION_RELATIONSHIP_WITH_TRANSFORMATION(#31)
SHAPE_REPRESENTATION_RELATIONSHIP()
);
#137=(
REPRESENTATION_RELATIONSHIP($,$,#20317,#20313)
REPRESENTATION_RELATIONSHIP_WITH_TRANSFORMATION(#32)
SHAPE_REPRESENTATION_RELATIONSHIP()
);
#138=(
REPRESENTATION_RELATIONSHIP($,$,#20318,#20313)
REPRESENTATION_RELATIONSHIP_WITH_TRANSFORMATION(#33)
SHAPE_REPRESENTATION_RELATIONSHIP()
);
#139=(
REPRESENTATION_RELATIONSHIP($,$,#20319,#20313)
REPRESENTATION_RELATIONSHIP_WITH_TRANSFORMATION(#34)
SHAPE_REPRESENTATION_RELATIONSHIP()
);
#140=(
REPRESENTATION_RELATIONSHIP($,$,#20320,#20313)
REPRESENTATION_RELATIONSHIP_WITH_TRANSFORMATION(#35)
SHAPE_REPRESENTATION_RELATIONSHIP()
);
#141=(
REPRESENTATION_RELATIONSHIP($,$,#20321,#20313)
REPRESENTATION_RELATIONSHIP_WITH_TRANSFORMATION(#36)
SHAPE_REPRESENTATION_RELATIONSHIP()
);
#142=(
REPRESENTATION_RELATIONSHIP($,$,#20322,#20313)
REPRESENTATION_RELATIONSHIP_WITH_TRANSFORMATION(#37)
SHAPE_REPRESENTATION_RELATIONSHIP()
);
#143=(
REPRESENTATION_RELATIONSHIP($,$,#20323,#20313)
REPRESENTATION_RELATIONSHIP_WITH_TRANSFORMATION(#38)
SHAPE_REPRESENTATION_RELATIONSHIP()
);
#144=(
REPRESENTATION_RELATIONSHIP($,$,#20324,#20313)
REPRESENTATION_RELATIONSHIP_WITH_TRANSFORMATION(#39)
SHAPE_REPRESENTATION_RELATIONSHIP()
);
#145=(
REPRESENTATION_RELATIONSHIP($,$,#20325,#20313)
REPRESENTATION_RELATIONSHIP_WITH_TRANSFORMATION(#40)
SHAPE_REPRESENTATION_RELATIONSHIP()
);
#146=(
REPRESENTATION_RELATIONSHIP($,$,#20326,#20313)
REPRESENTATION_RELATIONSHIP_WITH_TRANSFORMATION(#41)
SHAPE_REPRESENTATION_RELATIONSHIP()
);
#147=(
REPRESENTATION_RELATIONSHIP($,$,#20327,#20313)
REPRESENTATION_RELATIONSHIP_WITH_TRANSFORMATION(#42)
SHAPE_REPRESENTATION_RELATIONSHIP()
);
#148=(
REPRESENTATION_RELATIONSHIP($,$,#20364,#20313)
REPRESENTATION_RELATIONSHIP_WITH_TRANSFORMATION(#43)
SHAPE_REPRESENTATION_RELATIONSHIP()
);
#149=(
REPRESENTATION_RELATIONSHIP($,$,#20364,#20313)
REPRESENTATION_RELATIONSHIP_WITH_TRANSFORMATION(#44)
SHAPE_REPRESENTATION_RELATIONSHIP()
);
#150=(
REPRESENTATION_RELATIONSHIP($,$,#20364,#20313)
REPRESENTATION_RELATIONSHIP_WITH_TRANSFORMATION(#45)
SHAPE_REPRESENTATION_RELATIONSHIP()
);
#151=(
REPRESENTATION_RELATIONSHIP($,$,#20364,#20313)
REPRESENTATION_RELATIONSHIP_WITH_TRANSFORMATION(#46)
SHAPE_REPRESENTATION_RELATIONSHIP()
);
#152=(
REPRESENTATION_RELATIONSHIP($,$,#20328,#20313)
REPRESENTATION_RELATIONSHIP_WITH_TRANSFORMATION(#47)
SHAPE_REPRESENTATION_RELATIONSHIP()
);
#153=(
REPRESENTATION_RELATIONSHIP($,$,#20328,#20313)
REPRESENTATION_RELATIONSHIP_WITH_TRANSFORMATION(#48)
SHAPE_REPRESENTATION_RELATIONSHIP()
);
#154=(
REPRESENTATION_RELATIONSHIP($,$,#20363,#20313)
REPRESENTATION_RELATIONSHIP_WITH_TRANSFORMATION(#49)
SHAPE_REPRESENTATION_RELATIONSHIP()
);
#155=(
REPRESENTATION_RELATIONSHIP($,$,#20363,#20313)
REPRESENTATION_RELATIONSHIP_WITH_TRANSFORMATION(#50)
SHAPE_REPRESENTATION_RELATIONSHIP()
);
#156=(
REPRESENTATION_RELATIONSHIP($,$,#20363,#20313)
REPRESENTATION_RELATIONSHIP_WITH_TRANSFORMATION(#51)
SHAPE_REPRESENTATION_RELATIONSHIP()
);
#157=(
REPRESENTATION_RELATIONSHIP($,$,#20363,#20313)
REPRESENTATION_RELATIONSHIP_WITH_TRANSFORMATION(#52)
SHAPE_REPRESENTATION_RELATIONSHIP()
);
#158=(
REPRESENTATION_RELATIONSHIP($,$,#20363,#20313)
REPRESENTATION_RELATIONSHIP_WITH_TRANSFORMATION(#53)
SHAPE_REPRESENTATION_RELATIONSHIP()
);
#159=(
REPRESENTATION_RELATIONSHIP($,$,#20363,#20313)
REPRESENTATION_RELATIONSHIP_WITH_TRANSFORMATION(#54)
SHAPE_REPRESENTATION_RELATIONSHIP()
);
#160=(
REPRESENTATION_RELATIONSHIP($,$,#20363,#20313)
REPRESENTATION_RELATIONSHIP_WITH_TRANSFORMATION(#55)
SHAPE_REPRESENTATION_RELATIONSHIP()
);
#161=(
REPRESENTATION_RELATIONSHIP($,$,#20363,#20313)
REPRESENTATION_RELATIONSHIP_WITH_TRANSFORMATION(#56)
SHAPE_REPRESENTATION_RELATIONSHIP()
);
#162=(
REPRESENTATION_RELATIONSHIP($,$,#20364,#20313)
REPRESENTATION_RELATIONSHIP_WITH_TRANSFORMATION(#57)
SHAPE_REPRESENTATION_RELATIONSHIP()
);
#163=(
REPRESENTATION_RELATIONSHIP($,$,#20364,#20313)
REPRESENTATION_RELATIONSHIP_WITH_TRANSFORMATION(#58)
SHAPE_REPRESENTATION_RELATIONSHIP()
);
#164=(
REPRESENTATION_RELATIONSHIP($,$,#20364,#20313)
REPRESENTATION_RELATIONSHIP_WITH_TRANSFORMATION(#59)
SHAPE_REPRESENTATION_RELATIONSHIP()
);
#165=(
REPRESENTATION_RELATIONSHIP($,$,#20364,#20313)
REPRESENTATION_RELATIONSHIP_WITH_TRANSFORMATION(#60)
SHAPE_REPRESENTATION_RELATIONSHIP()
);
#166=(
REPRESENTATION_RELATIONSHIP($,$,#20328,#20313)
REPRESENTATION_RELATIONSHIP_WITH_TRANSFORMATION(#61)
SHAPE_REPRESENTATION_RELATIONSHIP()
);
#167=(
REPRESENTATION_RELATIONSHIP($,$,#20328,#20313)
REPRESENTATION_RELATIONSHIP_WITH_TRANSFORMATION(#62)
SHAPE_REPRESENTATION_RELATIONSHIP()
);
#168=(
REPRESENTATION_RELATIONSHIP($,$,#20363,#20313)
REPRESENTATION_RELATIONSHIP_WITH_TRANSFORMATION(#63)
SHAPE_REPRESENTATION_RELATIONSHIP()
);
#169=(
REPRESENTATION_RELATIONSHIP($,$,#20363,#20313)
REPRESENTATION_RELATIONSHIP_WITH_TRANSFORMATION(#64)
SHAPE_REPRESENTATION_RELATIONSHIP()
);
#170=(
REPRESENTATION_RELATIONSHIP($,$,#20363,#20313)
REPRESENTATION_RELATIONSHIP_WITH_TRANSFORMATION(#65)
SHAPE_REPRESENTATION_RELATIONSHIP()
);
#171=(
REPRESENTATION_RELATIONSHIP($,$,#20363,#20313)
REPRESENTATION_RELATIONSHIP_WITH_TRANSFORMATION(#66)
SHAPE_REPRESENTATION_RELATIONSHIP()
);
#172=(
REPRESENTATION_RELATIONSHIP($,$,#20363,#20313)
REPRESENTATION_RELATIONSHIP_WITH_TRANSFORMATION(#67)
SHAPE_REPRESENTATION_RELATIONSHIP()
);
#173=(
REPRESENTATION_RELATIONSHIP($,$,#20363,#20313)
REPRESENTATION_RELATIONSHIP_WITH_TRANSFORMATION(#68)
SHAPE_REPRESENTATION_RELATIONSHIP()
);
#174=(
REPRESENTATION_RELATIONSHIP($,$,#20363,#20313)
REPRESENTATION_RELATIONSHIP_WITH_TRANSFORMATION(#69)
SHAPE_REPRESENTATION_RELATIONSHIP()
);
#175=(
REPRESENTATION_RELATIONSHIP($,$,#20363,#20313)
REPRESENTATION_RELATIONSHIP_WITH_TRANSFORMATION(#70)
SHAPE_REPRESENTATION_RELATIONSHIP()
);
#176=(
REPRESENTATION_RELATIONSHIP($,$,#20334,#20313)
REPRESENTATION_RELATIONSHIP_WITH_TRANSFORMATION(#71)
SHAPE_REPRESENTATION_RELATIONSHIP()
);
#177=(
REPRESENTATION_RELATIONSHIP($,$,#20335,#20313)
REPRESENTATION_RELATIONSHIP_WITH_TRANSFORMATION(#72)
SHAPE_REPRESENTATION_RELATIONSHIP()
);
#178=(
REPRESENTATION_RELATIONSHIP($,$,#20336,#20313)
REPRESENTATION_RELATIONSHIP_WITH_TRANSFORMATION(#73)
SHAPE_REPRESENTATION_RELATIONSHIP()
);
#179=(
REPRESENTATION_RELATIONSHIP($,$,#20335,#20313)
REPRESENTATION_RELATIONSHIP_WITH_TRANSFORMATION(#74)
SHAPE_REPRESENTATION_RELATIONSHIP()
);
#180=(
REPRESENTATION_RELATIONSHIP($,$,#20336,#20313)
REPRESENTATION_RELATIONSHIP_WITH_TRANSFORMATION(#75)
SHAPE_REPRESENTATION_RELATIONSHIP()
);
#181=(
REPRESENTATION_RELATIONSHIP($,$,#20334,#20313)
REPRESENTATION_RELATIONSHIP_WITH_TRANSFORMATION(#76)
SHAPE_REPRESENTATION_RELATIONSHIP()
);
#182=(
REPRESENTATION_RELATIONSHIP($,$,#20335,#20313)
REPRESENTATION_RELATIONSHIP_WITH_TRANSFORMATION(#77)
SHAPE_REPRESENTATION_RELATIONSHIP()
);
#183=(
REPRESENTATION_RELATIONSHIP($,$,#20336,#20313)
REPRESENTATION_RELATIONSHIP_WITH_TRANSFORMATION(#78)
SHAPE_REPRESENTATION_RELATIONSHIP()
);
#184=(
REPRESENTATION_RELATIONSHIP($,$,#20335,#20313)
REPRESENTATION_RELATIONSHIP_WITH_TRANSFORMATION(#79)
SHAPE_REPRESENTATION_RELATIONSHIP()
);
#185=(
REPRESENTATION_RELATIONSHIP($,$,#20336,#20313)
REPRESENTATION_RELATIONSHIP_WITH_TRANSFORMATION(#80)
SHAPE_REPRESENTATION_RELATIONSHIP()
);
#186=(
REPRESENTATION_RELATIONSHIP($,$,#20337,#20313)
REPRESENTATION_RELATIONSHIP_WITH_TRANSFORMATION(#81)
SHAPE_REPRESENTATION_RELATIONSHIP()
);
#187=(
REPRESENTATION_RELATIONSHIP($,$,#20364,#20313)
REPRESENTATION_RELATIONSHIP_WITH_TRANSFORMATION(#82)
SHAPE_REPRESENTATION_RELATIONSHIP()
);
#188=(
REPRESENTATION_RELATIONSHIP($,$,#20364,#20313)
REPRESENTATION_RELATIONSHIP_WITH_TRANSFORMATION(#83)
SHAPE_REPRESENTATION_RELATIONSHIP()
);
#189=(
REPRESENTATION_RELATIONSHIP($,$,#20364,#20313)
REPRESENTATION_RELATIONSHIP_WITH_TRANSFORMATION(#84)
SHAPE_REPRESENTATION_RELATIONSHIP()
);
#190=(
REPRESENTATION_RELATIONSHIP($,$,#20364,#20313)
REPRESENTATION_RELATIONSHIP_WITH_TRANSFORMATION(#85)
SHAPE_REPRESENTATION_RELATIONSHIP()
);
#191=(
REPRESENTATION_RELATIONSHIP($,$,#20364,#20313)
REPRESENTATION_RELATIONSHIP_WITH_TRANSFORMATION(#86)
SHAPE_REPRESENTATION_RELATIONSHIP()
);
#192=(
REPRESENTATION_RELATIONSHIP($,$,#20364,#20313)
REPRESENTATION_RELATIONSHIP_WITH_TRANSFORMATION(#87)
SHAPE_REPRESENTATION_RELATIONSHIP()
);
#193=(
REPRESENTATION_RELATIONSHIP($,$,#20364,#20313)
REPRESENTATION_RELATIONSHIP_WITH_TRANSFORMATION(#88)
SHAPE_REPRESENTATION_RELATIONSHIP()
);
#194=(
REPRESENTATION_RELATIONSHIP($,$,#20364,#20313)
REPRESENTATION_RELATIONSHIP_WITH_TRANSFORMATION(#89)
SHAPE_REPRESENTATION_RELATIONSHIP()
);
#195=(
REPRESENTATION_RELATIONSHIP($,$,#20339,#20338)
REPRESENTATION_RELATIONSHIP_WITH_TRANSFORMATION(#90)
SHAPE_REPRESENTATION_RELATIONSHIP()
);
#196=(
REPRESENTATION_RELATIONSHIP($,$,#20340,#20338)
REPRESENTATION_RELATIONSHIP_WITH_TRANSFORMATION(#91)
SHAPE_REPRESENTATION_RELATIONSHIP()
);
#197=(
REPRESENTATION_RELATIONSHIP($,$,#20341,#20338)
REPRESENTATION_RELATIONSHIP_WITH_TRANSFORMATION(#92)
SHAPE_REPRESENTATION_RELATIONSHIP()
);
#198=(
REPRESENTATION_RELATIONSHIP($,$,#20342,#20338)
REPRESENTATION_RELATIONSHIP_WITH_TRANSFORMATION(#93)
SHAPE_REPRESENTATION_RELATIONSHIP()
);
#199=(
REPRESENTATION_RELATIONSHIP($,$,#20343,#20338)
REPRESENTATION_RELATIONSHIP_WITH_TRANSFORMATION(#94)
SHAPE_REPRESENTATION_RELATIONSHIP()
);
#200=(
REPRESENTATION_RELATIONSHIP($,$,#20344,#20338)
REPRESENTATION_RELATIONSHIP_WITH_TRANSFORMATION(#95)
SHAPE_REPRESENTATION_RELATIONSHIP()
);
#201=(
REPRESENTATION_RELATIONSHIP($,$,#20352,#20338)
REPRESENTATION_RELATIONSHIP_WITH_TRANSFORMATION(#96)
SHAPE_REPRESENTATION_RELATIONSHIP()
);
#202=(
REPRESENTATION_RELATIONSHIP($,$,#20364,#20338)
REPRESENTATION_RELATIONSHIP_WITH_TRANSFORMATION(#97)
SHAPE_REPRESENTATION_RELATIONSHIP()
);
#203=(
REPRESENTATION_RELATIONSHIP($,$,#20346,#20345)
REPRESENTATION_RELATIONSHIP_WITH_TRANSFORMATION(#98)
SHAPE_REPRESENTATION_RELATIONSHIP()
);
#204=(
REPRESENTATION_RELATIONSHIP($,$,#20347,#20345)
REPRESENTATION_RELATIONSHIP_WITH_TRANSFORMATION(#99)
SHAPE_REPRESENTATION_RELATIONSHIP()
);
#205=(
REPRESENTATION_RELATIONSHIP($,$,#20348,#20345)
REPRESENTATION_RELATIONSHIP_WITH_TRANSFORMATION(#100)
SHAPE_REPRESENTATION_RELATIONSHIP()
);
#206=(
REPRESENTATION_RELATIONSHIP($,$,#20349,#20345)
REPRESENTATION_RELATIONSHIP_WITH_TRANSFORMATION(#101)
SHAPE_REPRESENTATION_RELATIONSHIP()
);
#207=(
REPRESENTATION_RELATIONSHIP($,$,#20350,#20345)
REPRESENTATION_RELATIONSHIP_WITH_TRANSFORMATION(#102)
SHAPE_REPRESENTATION_RELATIONSHIP()
);
#208=(
REPRESENTATION_RELATIONSHIP($,$,#20351,#20345)
REPRESENTATION_RELATIONSHIP_WITH_TRANSFORMATION(#103)
SHAPE_REPRESENTATION_RELATIONSHIP()
);
#209=(
REPRESENTATION_RELATIONSHIP($,$,#20352,#20345)
REPRESENTATION_RELATIONSHIP_WITH_TRANSFORMATION(#104)
SHAPE_REPRESENTATION_RELATIONSHIP()
);
#210=(
REPRESENTATION_RELATIONSHIP($,$,#20364,#20345)
REPRESENTATION_RELATIONSHIP_WITH_TRANSFORMATION(#105)
SHAPE_REPRESENTATION_RELATIONSHIP()
);
#211=(
REPRESENTATION_RELATIONSHIP($,$,#20354,#20353)
REPRESENTATION_RELATIONSHIP_WITH_TRANSFORMATION(#106)
SHAPE_REPRESENTATION_RELATIONSHIP()
);
#212=(
REPRESENTATION_RELATIONSHIP($,$,#20355,#20353)
REPRESENTATION_RELATIONSHIP_WITH_TRANSFORMATION(#107)
SHAPE_REPRESENTATION_RELATIONSHIP()
);
#213=(
REPRESENTATION_RELATIONSHIP($,$,#20356,#20353)
REPRESENTATION_RELATIONSHIP_WITH_TRANSFORMATION(#108)
SHAPE_REPRESENTATION_RELATIONSHIP()
);
#214=(
REPRESENTATION_RELATIONSHIP($,$,#20357,#20353)
REPRESENTATION_RELATIONSHIP_WITH_TRANSFORMATION(#109)
SHAPE_REPRESENTATION_RELATIONSHIP()
);
#215=(
REPRESENTATION_RELATIONSHIP($,$,#20361,#20353)
REPRESENTATION_RELATIONSHIP_WITH_TRANSFORMATION(#110)
SHAPE_REPRESENTATION_RELATIONSHIP()
);
#216=(
REPRESENTATION_RELATIONSHIP($,$,#20362,#20353)
REPRESENTATION_RELATIONSHIP_WITH_TRANSFORMATION(#111)
SHAPE_REPRESENTATION_RELATIONSHIP()
);
#217=(
REPRESENTATION_RELATIONSHIP($,$,#20361,#20353)
REPRESENTATION_RELATIONSHIP_WITH_TRANSFORMATION(#112)
SHAPE_REPRESENTATION_RELATIONSHIP()
);
#218=(
REPRESENTATION_RELATIONSHIP($,$,#20362,#20353)
REPRESENTATION_RELATIONSHIP_WITH_TRANSFORMATION(#113)
SHAPE_REPRESENTATION_RELATIONSHIP()
);
#219=(
REPRESENTATION_RELATIONSHIP($,$,#20361,#20353)
REPRESENTATION_RELATIONSHIP_WITH_TRANSFORMATION(#114)
SHAPE_REPRESENTATION_RELATIONSHIP()
);
#220=(
REPRESENTATION_RELATIONSHIP($,$,#20362,#20353)
REPRESENTATION_RELATIONSHIP_WITH_TRANSFORMATION(#115)
SHAPE_REPRESENTATION_RELATIONSHIP()
);
#221=(
REPRESENTATION_RELATIONSHIP($,$,#20361,#20353)
REPRESENTATION_RELATIONSHIP_WITH_TRANSFORMATION(#116)
SHAPE_REPRESENTATION_RELATIONSHIP()
);
#222=(
REPRESENTATION_RELATIONSHIP($,$,#20362,#20353)
REPRESENTATION_RELATIONSHIP_WITH_TRANSFORMATION(#117)
SHAPE_REPRESENTATION_RELATIONSHIP()
);
#223=(
REPRESENTATION_RELATIONSHIP($,$,#20363,#20353)
REPRESENTATION_RELATIONSHIP_WITH_TRANSFORMATION(#118)
SHAPE_REPRESENTATION_RELATIONSHIP()
);
#224=(
REPRESENTATION_RELATIONSHIP($,$,#20363,#20353)
REPRESENTATION_RELATIONSHIP_WITH_TRANSFORMATION(#119)
SHAPE_REPRESENTATION_RELATIONSHIP()
);
#225=(
REPRESENTATION_RELATIONSHIP($,$,#20364,#20353)
REPRESENTATION_RELATIONSHIP_WITH_TRANSFORMATION(#120)
SHAPE_REPRESENTATION_RELATIONSHIP()
);
#226=(
REPRESENTATION_RELATIONSHIP($,$,#20364,#20353)
REPRESENTATION_RELATIONSHIP_WITH_TRANSFORMATION(#121)
SHAPE_REPRESENTATION_RELATIONSHIP()
);
#227=(
REPRESENTATION_RELATIONSHIP($,$,#20313,#20312)
REPRESENTATION_RELATIONSHIP_WITH_TRANSFORMATION(#122)
SHAPE_REPRESENTATION_RELATIONSHIP()
);
#228=(
REPRESENTATION_RELATIONSHIP($,$,#20338,#20312)
REPRESENTATION_RELATIONSHIP_WITH_TRANSFORMATION(#123)
SHAPE_REPRESENTATION_RELATIONSHIP()
);
#229=(
REPRESENTATION_RELATIONSHIP($,$,#20345,#20312)
REPRESENTATION_RELATIONSHIP_WITH_TRANSFORMATION(#124)
SHAPE_REPRESENTATION_RELATIONSHIP()
);
#230=(
REPRESENTATION_RELATIONSHIP($,$,#20353,#20312)
REPRESENTATION_RELATIONSHIP_WITH_TRANSFORMATION(#125)
SHAPE_REPRESENTATION_RELATIONSHIP()
);
#231=CONTEXT_DEPENDENT_SHAPE_REPRESENTATION(#126,#20176);
#232=CONTEXT_DEPENDENT_SHAPE_REPRESENTATION(#127,#20177);
#233=CONTEXT_DEPENDENT_SHAPE_REPRESENTATION(#128,#20178);
#234=CONTEXT_DEPENDENT_SHAPE_REPRESENTATION(#129,#20179);
#235=CONTEXT_DEPENDENT_SHAPE_REPRESENTATION(#130,#20180);
#236=CONTEXT_DEPENDENT_SHAPE_REPRESENTATION(#131,#20208);
#237=CONTEXT_DEPENDENT_SHAPE_REPRESENTATION(#132,#20209);
#238=CONTEXT_DEPENDENT_SHAPE_REPRESENTATION(#133,#20210);
#239=CONTEXT_DEPENDENT_SHAPE_REPRESENTATION(#134,#20215);
#240=CONTEXT_DEPENDENT_SHAPE_REPRESENTATION(#135,#20216);
#241=CONTEXT_DEPENDENT_SHAPE_REPRESENTATION(#136,#20217);
#242=CONTEXT_DEPENDENT_SHAPE_REPRESENTATION(#137,#20218);
#243=CONTEXT_DEPENDENT_SHAPE_REPRESENTATION(#138,#20219);
#244=CONTEXT_DEPENDENT_SHAPE_REPRESENTATION(#139,#20220);
#245=CONTEXT_DEPENDENT_SHAPE_REPRESENTATION(#140,#20221);
#246=CONTEXT_DEPENDENT_SHAPE_REPRESENTATION(#141,#20222);
#247=CONTEXT_DEPENDENT_SHAPE_REPRESENTATION(#142,#20223);
#248=CONTEXT_DEPENDENT_SHAPE_REPRESENTATION(#143,#20224);
#249=CONTEXT_DEPENDENT_SHAPE_REPRESENTATION(#144,#20225);
#250=CONTEXT_DEPENDENT_SHAPE_REPRESENTATION(#145,#20226);
#251=CONTEXT_DEPENDENT_SHAPE_REPRESENTATION(#146,#20227);
#252=CONTEXT_DEPENDENT_SHAPE_REPRESENTATION(#147,#20228);
#253=CONTEXT_DEPENDENT_SHAPE_REPRESENTATION(#148,#20229);
#254=CONTEXT_DEPENDENT_SHAPE_REPRESENTATION(#149,#20230);
#255=CONTEXT_DEPENDENT_SHAPE_REPRESENTATION(#150,#20231);
#256=CONTEXT_DEPENDENT_SHAPE_REPRESENTATION(#151,#20232);
#257=CONTEXT_DEPENDENT_SHAPE_REPRESENTATION(#152,#20233);
#258=CONTEXT_DEPENDENT_SHAPE_REPRESENTATION(#153,#20234);
#259=CONTEXT_DEPENDENT_SHAPE_REPRESENTATION(#154,#20235);
#260=CONTEXT_DEPENDENT_SHAPE_REPRESENTATION(#155,#20236);
#261=CONTEXT_DEPENDENT_SHAPE_REPRESENTATION(#156,#20237);
#262=CONTEXT_DEPENDENT_SHAPE_REPRESENTATION(#157,#20238);
#263=CONTEXT_DEPENDENT_SHAPE_REPRESENTATION(#158,#20239);
#264=CONTEXT_DEPENDENT_SHAPE_REPRESENTATION(#159,#20240);
#265=CONTEXT_DEPENDENT_SHAPE_REPRESENTATION(#160,#20241);
#266=CONTEXT_DEPENDENT_SHAPE_REPRESENTATION(#161,#20242);
#267=CONTEXT_DEPENDENT_SHAPE_REPRESENTATION(#162,#20243);
#268=CONTEXT_DEPENDENT_SHAPE_REPRESENTATION(#163,#20244);
#269=CONTEXT_DEPENDENT_SHAPE_REPRESENTATION(#164,#20245);
#270=CONTEXT_DEPENDENT_SHAPE_REPRESENTATION(#165,#20246);
#271=CONTEXT_DEPENDENT_SHAPE_REPRESENTATION(#166,#20247);
#272=CONTEXT_DEPENDENT_SHAPE_REPRESENTATION(#167,#20248);
#273=CONTEXT_DEPENDENT_SHAPE_REPRESENTATION(#168,#20249);
#274=CONTEXT_DEPENDENT_SHAPE_REPRESENTATION(#169,#20250);
#275=CONTEXT_DEPENDENT_SHAPE_REPRESENTATION(#170,#20251);
#276=CONTEXT_DEPENDENT_SHAPE_REPRESENTATION(#171,#20252);
#277=CONTEXT_DEPENDENT_SHAPE_REPRESENTATION(#172,#20253);
#278=CONTEXT_DEPENDENT_SHAPE_REPRESENTATION(#173,#20254);
#279=CONTEXT_DEPENDENT_SHAPE_REPRESENTATION(#174,#20255);
#280=CONTEXT_DEPENDENT_SHAPE_REPRESENTATION(#175,#20256);
#281=CONTEXT_DEPENDENT_SHAPE_REPRESENTATION(#176,#20257);
#282=CONTEXT_DEPENDENT_SHAPE_REPRESENTATION(#177,#20258);
#283=CONTEXT_DEPENDENT_SHAPE_REPRESENTATION(#178,#20259);
#284=CONTEXT_DEPENDENT_SHAPE_REPRESENTATION(#179,#20260);
#285=CONTEXT_DEPENDENT_SHAPE_REPRESENTATION(#180,#20261);
#286=CONTEXT_DEPENDENT_SHAPE_REPRESENTATION(#181,#20262);
#287=CONTEXT_DEPENDENT_SHAPE_REPRESENTATION(#182,#20263);
#288=CONTEXT_DEPENDENT_SHAPE_REPRESENTATION(#183,#20264);
#289=CONTEXT_DEPENDENT_SHAPE_REPRESENTATION(#184,#20265);
#290=CONTEXT_DEPENDENT_SHAPE_REPRESENTATION(#185,#20266);
#291=CONTEXT_DEPENDENT_SHAPE_REPRESENTATION(#186,#20267);
#292=CONTEXT_DEPENDENT_SHAPE_REPRESENTATION(#187,#20268);
#293=CONTEXT_DEPENDENT_SHAPE_REPRESENTATION(#188,#20269);
#294=CONTEXT_DEPENDENT_SHAPE_REPRESENTATION(#189,#20270);
#295=CONTEXT_DEPENDENT_SHAPE_REPRESENTATION(#190,#20271);
#296=CONTEXT_DEPENDENT_SHAPE_REPRESENTATION(#191,#20272);
#297=CONTEXT_DEPENDENT_SHAPE_REPRESENTATION(#192,#20273);
#298=CONTEXT_DEPENDENT_SHAPE_REPRESENTATION(#193,#20274);
#299=CONTEXT_DEPENDENT_SHAPE_REPRESENTATION(#194,#20275);
#300=CONTEXT_DEPENDENT_SHAPE_REPRESENTATION(#195,#20276);
#301=CONTEXT_DEPENDENT_SHAPE_REPRESENTATION(#196,#20277);
#302=CONTEXT_DEPENDENT_SHAPE_REPRESENTATION(#197,#20278);
#303=CONTEXT_DEPENDENT_SHAPE_REPRESENTATION(#198,#20279);
#304=CONTEXT_DEPENDENT_SHAPE_REPRESENTATION(#199,#20280);
#305=CONTEXT_DEPENDENT_SHAPE_REPRESENTATION(#200,#20281);
#306=CONTEXT_DEPENDENT_SHAPE_REPRESENTATION(#201,#20282);
#307=CONTEXT_DEPENDENT_SHAPE_REPRESENTATION(#202,#20283);
#308=CONTEXT_DEPENDENT_SHAPE_REPRESENTATION(#203,#20284);
#309=CONTEXT_DEPENDENT_SHAPE_REPRESENTATION(#204,#20285);
#310=CONTEXT_DEPENDENT_SHAPE_REPRESENTATION(#205,#20286);
#311=CONTEXT_DEPENDENT_SHAPE_REPRESENTATION(#206,#20287);
#312=CONTEXT_DEPENDENT_SHAPE_REPRESENTATION(#207,#20288);
#313=CONTEXT_DEPENDENT_SHAPE_REPRESENTATION(#208,#20289);
#314=CONTEXT_DEPENDENT_SHAPE_REPRESENTATION(#209,#20290);
#315=CONTEXT_DEPENDENT_SHAPE_REPRESENTATION(#210,#20291);
#316=CONTEXT_DEPENDENT_SHAPE_REPRESENTATION(#211,#20292);
#317=CONTEXT_DEPENDENT_SHAPE_REPRESENTATION(#212,#20293);
#318=CONTEXT_DEPENDENT_SHAPE_REPRESENTATION(#213,#20294);
#319=CONTEXT_DEPENDENT_SHAPE_REPRESENTATION(#214,#20295);
#320=CONTEXT_DEPENDENT_SHAPE_REPRESENTATION(#215,#20296);
#321=CONTEXT_DEPENDENT_SHAPE_REPRESENTATION(#216,#20297);
#322=CONTEXT_DEPENDENT_SHAPE_REPRESENTATION(#217,#20298);
#323=CONTEXT_DEPENDENT_SHAPE_REPRESENTATION(#218,#20299);
#324=CONTEXT_DEPENDENT_SHAPE_REPRESENTATION(#219,#20300);
#325=CONTEXT_DEPENDENT_SHAPE_REPRESENTATION(#220,#20301);
#326=CONTEXT_DEPENDENT_SHAPE_REPRESENTATION(#221,#20302);
#327=CONTEXT_DEPENDENT_SHAPE_REPRESENTATION(#222,#20303);
#328=CONTEXT_DEPENDENT_SHAPE_REPRESENTATION(#223,#20304);
#329=CONTEXT_DEPENDENT_SHAPE_REPRESENTATION(#224,#20305);
#330=CONTEXT_DEPENDENT_SHAPE_REPRESENTATION(#225,#20306);
#331=CONTEXT_DEPENDENT_SHAPE_REPRESENTATION(#226,#20307);
#332=CONTEXT_DEPENDENT_SHAPE_REPRESENTATION(#227,#20308);
#333=CONTEXT_DEPENDENT_SHAPE_REPRESENTATION(#228,#20309);
#334=CONTEXT_DEPENDENT_SHAPE_REPRESENTATION(#229,#20310);
#335=CONTEXT_DEPENDENT_SHAPE_REPRESENTATION(#230,#20311);
#336=NEXT_ASSEMBLY_USAGE_OCCURRENCE('Inner ring:1','Inner ring:1',
'Inner ring:1',#20382,#20383,'Inner ring:1');
#337=NEXT_ASSEMBLY_USAGE_OCCURRENCE('Outer ring:1','Outer ring:1',
'Outer ring:1',#20382,#20384,'Outer ring:1');
#338=NEXT_ASSEMBLY_USAGE_OCCURRENCE('Balls:1','Balls:1','Balls:1',#20382,
#20385,'Balls:1');
#339=NEXT_ASSEMBLY_USAGE_OCCURRENCE('Cage:1','Cage:1','Cage:1',#20382,#20386,
'Cage:1');
#340=NEXT_ASSEMBLY_USAGE_OCCURRENCE('Seals 2RS:1','Seals 2RS:1',
'Seals 2RS:1',#20382,#20387,'Seals 2RS:1');
#341=NEXT_ASSEMBLY_USAGE_OCCURRENCE('Block:1','Block:1','Block:1',#20411,
#20412,'Block:1');
#342=NEXT_ASSEMBLY_USAGE_OCCURRENCE('End cap +:1','End cap +:1',
'End cap +:1',#20411,#20413,'End cap +:1');
#343=NEXT_ASSEMBLY_USAGE_OCCURRENCE('End cap:1','End cap:1','End cap:1',
#20411,#20414,'End cap:1');
#344=NEXT_ASSEMBLY_USAGE_OCCURRENCE('Base:1','Base:1','Base:1',#20367,#20368,
'Base:1');
#345=NEXT_ASSEMBLY_USAGE_OCCURRENCE('Foot:1','Foot:1','Foot:1',#20367,#20369,
'Foot:1');
#346=NEXT_ASSEMBLY_USAGE_OCCURRENCE('Foot (1):1','Foot (1):1',
'Foot (1):1',#20367,#20370,'Foot (1):1');
#347=NEXT_ASSEMBLY_USAGE_OCCURRENCE('Fixed bearing block:1',
'Fixed bearing block:1','Fixed bearing block:1',#20367,#20371,
'Fixed bearing block:1');
#348=NEXT_ASSEMBLY_USAGE_OCCURRENCE('Input outer spacer:1',
'Input outer spacer:1','Input outer spacer:1',#20367,#20372,
'Input outer spacer:1');
#349=NEXT_ASSEMBLY_USAGE_OCCURRENCE('Input bearing cap:1',
'Input bearing cap:1','Input bearing cap:1',#20367,#20373,
'Input bearing cap:1');
#350=NEXT_ASSEMBLY_USAGE_OCCURRENCE('Input bearing cap (1):1',
'Input bearing cap (1):1','Input bearing cap (1):1',#20367,#20374,
'Input bearing cap (1):1');
#351=NEXT_ASSEMBLY_USAGE_OCCURRENCE('Fixed bearing block (1):1',
'Fixed bearing block (1):1','Fixed bearing block (1):1',#20367,#20375,
'Fixed bearing block (1):1');
#352=NEXT_ASSEMBLY_USAGE_OCCURRENCE('Input outer spacer (1):1',
'Input outer spacer (1):1','Input outer spacer (1):1',#20367,#20376,
'Input outer spacer (1):1');
#353=NEXT_ASSEMBLY_USAGE_OCCURRENCE('Input bearing cap (2):1',
'Input bearing cap (2):1','Input bearing cap (2):1',#20367,#20377,
'Input bearing cap (2):1');
#354=NEXT_ASSEMBLY_USAGE_OCCURRENCE('Input bearing cap (3):1',
'Input bearing cap (3):1','Input bearing cap (3):1',#20367,#20378,
'Input bearing cap (3):1');
#355=NEXT_ASSEMBLY_USAGE_OCCURRENCE('Timing belt backing envelope:1',
'Timing belt backing envelope:1','Timing belt backing envelope:1',#20367,
#20379,'Timing belt backing envelope:1');
#356=NEXT_ASSEMBLY_USAGE_OCCURRENCE('Travel stop:1','Travel stop:1',
'Travel stop:1',#20367,#20380,'Travel stop:1');
#357=NEXT_ASSEMBLY_USAGE_OCCURRENCE('Travel stop (1):1',
'Travel stop (1):1','Travel stop (1):1',#20367,#20381,
'Travel stop (1):1');
#358=NEXT_ASSEMBLY_USAGE_OCCURRENCE('Cap Screw - M4x16:2',
'Cap Screw - M4x16:2','Cap Screw - M4x16:2',#20367,#20418,
'Cap Screw - M4x16:2');
#359=NEXT_ASSEMBLY_USAGE_OCCURRENCE('Cap Screw - M4x16:3',
'Cap Screw - M4x16:3','Cap Screw - M4x16:3',#20367,#20418,
'Cap Screw - M4x16:3');
#360=NEXT_ASSEMBLY_USAGE_OCCURRENCE('Cap Screw - M4x16:4',
'Cap Screw - M4x16:4','Cap Screw - M4x16:4',#20367,#20418,
'Cap Screw - M4x16:4');
#361=NEXT_ASSEMBLY_USAGE_OCCURRENCE('Cap Screw - M4x16:5',
'Cap Screw - M4x16:5','Cap Screw - M4x16:5',#20367,#20418,
'Cap Screw - M4x16:5');
#362=NEXT_ASSEMBLY_USAGE_OCCURRENCE(
'Sealed Ball Bearing - 10 x 30 x 9 mm:2',
'Sealed Ball Bearing - 10 x 30 x 9 mm:2',
'Sealed Ball Bearing - 10 x 30 x 9 mm:2',#20367,#20382,
'Sealed Ball Bearing - 10 x 30 x 9 mm:2');
#363=NEXT_ASSEMBLY_USAGE_OCCURRENCE(
'Sealed Ball Bearing - 10 x 30 x 9 mm:3',
'Sealed Ball Bearing - 10 x 30 x 9 mm:3',
'Sealed Ball Bearing - 10 x 30 x 9 mm:3',#20367,#20382,
'Sealed Ball Bearing - 10 x 30 x 9 mm:3');
#364=NEXT_ASSEMBLY_USAGE_OCCURRENCE('M4x10 Cap Screw:2',
'M4x10 Cap Screw:2','M4x10 Cap Screw:2',#20367,#20417,
'M4x10 Cap Screw:2');
#365=NEXT_ASSEMBLY_USAGE_OCCURRENCE('M4x10 Cap Screw:3',
'M4x10 Cap Screw:3','M4x10 Cap Screw:3',#20367,#20417,
'M4x10 Cap Screw:3');
#366=NEXT_ASSEMBLY_USAGE_OCCURRENCE('M4x10 Cap Screw:4',
'M4x10 Cap Screw:4','M4x10 Cap Screw:4',#20367,#20417,
'M4x10 Cap Screw:4');
#367=NEXT_ASSEMBLY_USAGE_OCCURRENCE('M4x10 Cap Screw:5',
'M4x10 Cap Screw:5','M4x10 Cap Screw:5',#20367,#20417,
'M4x10 Cap Screw:5');
#368=NEXT_ASSEMBLY_USAGE_OCCURRENCE('M4x10 Cap Screw:6',
'M4x10 Cap Screw:6','M4x10 Cap Screw:6',#20367,#20417,
'M4x10 Cap Screw:6');
#369=NEXT_ASSEMBLY_USAGE_OCCURRENCE('M4x10 Cap Screw:7',
'M4x10 Cap Screw:7','M4x10 Cap Screw:7',#20367,#20417,
'M4x10 Cap Screw:7');
#370=NEXT_ASSEMBLY_USAGE_OCCURRENCE('M4x10 Cap Screw:8',
'M4x10 Cap Screw:8','M4x10 Cap Screw:8',#20367,#20417,
'M4x10 Cap Screw:8');
#371=NEXT_ASSEMBLY_USAGE_OCCURRENCE('M4x10 Cap Screw:9',
'M4x10 Cap Screw:9','M4x10 Cap Screw:9',#20367,#20417,
'M4x10 Cap Screw:9');
#372=NEXT_ASSEMBLY_USAGE_OCCURRENCE('Cap Screw - M4x16:7',
'Cap Screw - M4x16:7','Cap Screw - M4x16:7',#20367,#20418,
'Cap Screw - M4x16:7');
#373=NEXT_ASSEMBLY_USAGE_OCCURRENCE('Cap Screw - M4x16:8',
'Cap Screw - M4x16:8','Cap Screw - M4x16:8',#20367,#20418,
'Cap Screw - M4x16:8');
#374=NEXT_ASSEMBLY_USAGE_OCCURRENCE('Cap Screw - M4x16:9',
'Cap Screw - M4x16:9','Cap Screw - M4x16:9',#20367,#20418,
'Cap Screw - M4x16:9');
#375=NEXT_ASSEMBLY_USAGE_OCCURRENCE('Cap Screw - M4x16:10',
'Cap Screw - M4x16:10','Cap Screw - M4x16:10',#20367,#20418,
'Cap Screw - M4x16:10');
#376=NEXT_ASSEMBLY_USAGE_OCCURRENCE(
'Sealed Ball Bearing - 10 x 30 x 9 mm:4',
'Sealed Ball Bearing - 10 x 30 x 9 mm:4',
'Sealed Ball Bearing - 10 x 30 x 9 mm:4',#20367,#20382,
'Sealed Ball Bearing - 10 x 30 x 9 mm:4');
#377=NEXT_ASSEMBLY_USAGE_OCCURRENCE(
'Sealed Ball Bearing - 10 x 30 x 9 mm:5',
'Sealed Ball Bearing - 10 x 30 x 9 mm:5',
'Sealed Ball Bearing - 10 x 30 x 9 mm:5',#20367,#20382,
'Sealed Ball Bearing - 10 x 30 x 9 mm:5');
#378=NEXT_ASSEMBLY_USAGE_OCCURRENCE('M4x10 Cap Screw:10',
'M4x10 Cap Screw:10','M4x10 Cap Screw:10',#20367,#20417,
'M4x10 Cap Screw:10');
#379=NEXT_ASSEMBLY_USAGE_OCCURRENCE('M4x10 Cap Screw:11',
'M4x10 Cap Screw:11','M4x10 Cap Screw:11',#20367,#20417,
'M4x10 Cap Screw:11');
#380=NEXT_ASSEMBLY_USAGE_OCCURRENCE('M4x10 Cap Screw:12',
'M4x10 Cap Screw:12','M4x10 Cap Screw:12',#20367,#20417,
'M4x10 Cap Screw:12');
#381=NEXT_ASSEMBLY_USAGE_OCCURRENCE('M4x10 Cap Screw:13',
'M4x10 Cap Screw:13','M4x10 Cap Screw:13',#20367,#20417,
'M4x10 Cap Screw:13');
#382=NEXT_ASSEMBLY_USAGE_OCCURRENCE('M4x10 Cap Screw:14',
'M4x10 Cap Screw:14','M4x10 Cap Screw:14',#20367,#20417,
'M4x10 Cap Screw:14');
#383=NEXT_ASSEMBLY_USAGE_OCCURRENCE('M4x10 Cap Screw:15',
'M4x10 Cap Screw:15','M4x10 Cap Screw:15',#20367,#20417,
'M4x10 Cap Screw:15');
#384=NEXT_ASSEMBLY_USAGE_OCCURRENCE('M4x10 Cap Screw:16',
'M4x10 Cap Screw:16','M4x10 Cap Screw:16',#20367,#20417,
'M4x10 Cap Screw:16');
#385=NEXT_ASSEMBLY_USAGE_OCCURRENCE('M4x10 Cap Screw:17',
'M4x10 Cap Screw:17','M4x10 Cap Screw:17',#20367,#20417,
'M4x10 Cap Screw:17');
#386=NEXT_ASSEMBLY_USAGE_OCCURRENCE(
'Slotted Extrusion - 20 x 20 x 400 mm:2',
'Slotted Extrusion - 20 x 20 x 400 mm:2',
'Slotted Extrusion - 20 x 20 x 400 mm:2',#20367,#20388,
'Slotted Extrusion - 20 x 20 x 400 mm:2');
#387=NEXT_ASSEMBLY_USAGE_OCCURRENCE('Captive slot nut:2',
'Captive slot nut:2','Captive slot nut:2',#20367,#20389,
'Captive slot nut:2');
#388=NEXT_ASSEMBLY_USAGE_OCCURRENCE('M5x17.5 extrusion screw:2',
'M5x17.5 extrusion screw:2','M5x17.5 extrusion screw:2',#20367,#20390,
'M5x17.5 extrusion screw:2');
#389=NEXT_ASSEMBLY_USAGE_OCCURRENCE('Captive slot nut:3',
'Captive slot nut:3','Captive slot nut:3',#20367,#20389,
'Captive slot nut:3');
#390=NEXT_ASSEMBLY_USAGE_OCCURRENCE('M5x17.5 extrusion screw:3',
'M5x17.5 extrusion screw:3','M5x17.5 extrusion screw:3',#20367,#20390,
'M5x17.5 extrusion screw:3');
#391=NEXT_ASSEMBLY_USAGE_OCCURRENCE(
'Slotted Extrusion - 20 x 20 x 400 mm:3',
'Slotted Extrusion - 20 x 20 x 400 mm:3',
'Slotted Extrusion - 20 x 20 x 400 mm:3',#20367,#20388,
'Slotted Extrusion - 20 x 20 x 400 mm:3');
#392=NEXT_ASSEMBLY_USAGE_OCCURRENCE('Captive slot nut:4',
'Captive slot nut:4','Captive slot nut:4',#20367,#20389,
'Captive slot nut:4');
#393=NEXT_ASSEMBLY_USAGE_OCCURRENCE('M5x17.5 extrusion screw:4',
'M5x17.5 extrusion screw:4','M5x17.5 extrusion screw:4',#20367,#20390,
'M5x17.5 extrusion screw:4');
#394=NEXT_ASSEMBLY_USAGE_OCCURRENCE('Captive slot nut:5',
'Captive slot nut:5','Captive slot nut:5',#20367,#20389,
'Captive slot nut:5');
#395=NEXT_ASSEMBLY_USAGE_OCCURRENCE('M5x17.5 extrusion screw:5',
'M5x17.5 extrusion screw:5','M5x17.5 extrusion screw:5',#20367,#20390,
'M5x17.5 extrusion screw:5');
#396=NEXT_ASSEMBLY_USAGE_OCCURRENCE(
'Linear Guide Rail - 15 mm, 220 mm Long:2',
'Linear Guide Rail - 15 mm, 220 mm Long:2',
'Linear Guide Rail - 15 mm, 220 mm Long:2',#20367,#20391,
'Linear Guide Rail - 15 mm, 220 mm Long:2');
#397=NEXT_ASSEMBLY_USAGE_OCCURRENCE('Cap Screw - M4x16:12',
'Cap Screw - M4x16:12','Cap Screw - M4x16:12',#20367,#20418,
'Cap Screw - M4x16:12');
#398=NEXT_ASSEMBLY_USAGE_OCCURRENCE('Cap Screw - M4x16:13',
'Cap Screw - M4x16:13','Cap Screw - M4x16:13',#20367,#20418,
'Cap Screw - M4x16:13');
#399=NEXT_ASSEMBLY_USAGE_OCCURRENCE('Cap Screw - M4x16:14',
'Cap Screw - M4x16:14','Cap Screw - M4x16:14',#20367,#20418,
'Cap Screw - M4x16:14');
#400=NEXT_ASSEMBLY_USAGE_OCCURRENCE('Cap Screw - M4x16:15',
'Cap Screw - M4x16:15','Cap Screw - M4x16:15',#20367,#20418,
'Cap Screw - M4x16:15');
#401=NEXT_ASSEMBLY_USAGE_OCCURRENCE('Cap Screw - M4x16:18',
'Cap Screw - M4x16:18','Cap Screw - M4x16:18',#20367,#20418,
'Cap Screw - M4x16:18');
#402=NEXT_ASSEMBLY_USAGE_OCCURRENCE('Cap Screw - M4x16:19',
'Cap Screw - M4x16:19','Cap Screw - M4x16:19',#20367,#20418,
'Cap Screw - M4x16:19');
#403=NEXT_ASSEMBLY_USAGE_OCCURRENCE('Cap Screw - M4x16:20',
'Cap Screw - M4x16:20','Cap Screw - M4x16:20',#20367,#20418,
'Cap Screw - M4x16:20');
#404=NEXT_ASSEMBLY_USAGE_OCCURRENCE('Cap Screw - M4x16:21',
'Cap Screw - M4x16:21','Cap Screw - M4x16:21',#20367,#20418,
'Cap Screw - M4x16:21');
#405=NEXT_ASSEMBLY_USAGE_OCCURRENCE('Input shaft:1','Input shaft:1',
'Input shaft:1',#20392,#20393,'Input shaft:1');
#406=NEXT_ASSEMBLY_USAGE_OCCURRENCE('Input inner spacer:1',
'Input inner spacer:1','Input inner spacer:1',#20392,#20394,
'Input inner spacer:1');
#407=NEXT_ASSEMBLY_USAGE_OCCURRENCE('Input inner sleeve:1',
'Input inner sleeve:1','Input inner sleeve:1',#20392,#20395,
'Input inner sleeve:1');
#408=NEXT_ASSEMBLY_USAGE_OCCURRENCE('Input M3 set screw:1',
'Input M3 set screw:1','Input M3 set screw:1',#20392,#20396,
'Input M3 set screw:1');
#409=NEXT_ASSEMBLY_USAGE_OCCURRENCE('Input M3 set screw (1):1',
'Input M3 set screw (1):1','Input M3 set screw (1):1',#20392,#20397,
'Input M3 set screw (1):1');
#410=NEXT_ASSEMBLY_USAGE_OCCURRENCE('Input end keeper:1',
'Input end keeper:1','Input end keeper:1',#20392,#20398,
'Input end keeper:1');
#411=NEXT_ASSEMBLY_USAGE_OCCURRENCE(
'Timing Pulley - 2 mm Pitch, 20 Teeth, 8 mm Bore:2',
'Timing Pulley - 2 mm Pitch, 20 Teeth, 8 mm Bore:2',
'Timing Pulley - 2 mm Pitch, 20 Teeth, 8 mm Bore:2',#20392,#20406,
'Timing Pulley - 2 mm Pitch, 20 Teeth, 8 mm Bore:2');
#412=NEXT_ASSEMBLY_USAGE_OCCURRENCE('Cap Screw - M4x16:6',
'Cap Screw - M4x16:6','Cap Screw - M4x16:6',#20392,#20418,
'Cap Screw - M4x16:6');
#413=NEXT_ASSEMBLY_USAGE_OCCURRENCE('Input shaft (1):1',
'Input shaft (1):1','Input shaft (1):1',#20399,#20400,
'Input shaft (1):1');
#414=NEXT_ASSEMBLY_USAGE_OCCURRENCE('Input inner spacer (1):1',
'Input inner spacer (1):1','Input inner spacer (1):1',#20399,#20401,
'Input inner spacer (1):1');
#415=NEXT_ASSEMBLY_USAGE_OCCURRENCE('Input inner sleeve (1):1',
'Input inner sleeve (1):1','Input inner sleeve (1):1',#20399,#20402,
'Input inner sleeve (1):1');
#416=NEXT_ASSEMBLY_USAGE_OCCURRENCE('Input M3 set screw (2):1',
'Input M3 set screw (2):1','Input M3 set screw (2):1',#20399,#20403,
'Input M3 set screw (2):1');
#417=NEXT_ASSEMBLY_USAGE_OCCURRENCE('Input M3 set screw (3):1',
'Input M3 set screw (3):1','Input M3 set screw (3):1',#20399,#20404,
'Input M3 set screw (3):1');
#418=NEXT_ASSEMBLY_USAGE_OCCURRENCE('Input end keeper (1):1',
'Input end keeper (1):1','Input end keeper (1):1',#20399,#20405,
'Input end keeper (1):1');
#419=NEXT_ASSEMBLY_USAGE_OCCURRENCE(
'Timing Pulley - 2 mm Pitch, 20 Teeth, 8 mm Bore:3',
'Timing Pulley - 2 mm Pitch, 20 Teeth, 8 mm Bore:3',
'Timing Pulley - 2 mm Pitch, 20 Teeth, 8 mm Bore:3',#20399,#20406,
'Timing Pulley - 2 mm Pitch, 20 Teeth, 8 mm Bore:3');
#420=NEXT_ASSEMBLY_USAGE_OCCURRENCE('Cap Screw - M4x16:11',
'Cap Screw - M4x16:11','Cap Screw - M4x16:11',#20399,#20418,
'Cap Screw - M4x16:11');
#421=NEXT_ASSEMBLY_USAGE_OCCURRENCE('Moving table:1','Moving table:1',
'Moving table:1',#20407,#20408,'Moving table:1');
#422=NEXT_ASSEMBLY_USAGE_OCCURRENCE('Belt attachment bracket:1',
'Belt attachment bracket:1','Belt attachment bracket:1',#20407,#20409,
'Belt attachment bracket:1');
#423=NEXT_ASSEMBLY_USAGE_OCCURRENCE('Belt clamp jaw:1',
'Belt clamp jaw:1','Belt clamp jaw:1',#20407,#20410,'Belt clamp jaw:1');
#424=NEXT_ASSEMBLY_USAGE_OCCURRENCE(
'Flanged Linear Guide Carriage - 15 mm:2',
'Flanged Linear Guide Carriage - 15 mm:2',
'Flanged Linear Guide Carriage - 15 mm:2',#20407,#20411,
'Flanged Linear Guide Carriage - 15 mm:2');
#425=NEXT_ASSEMBLY_USAGE_OCCURRENCE('Flat Washer - M5:2',
'Flat Washer - M5:2','Flat Washer - M5:2',#20407,#20415,
'Flat Washer - M5:2');
#426=NEXT_ASSEMBLY_USAGE_OCCURRENCE('Cap Screw - M5x20:2',
'Cap Screw - M5x20:2','Cap Screw - M5x20:2',#20407,#20416,
'Cap Screw - M5x20:2');
#427=NEXT_ASSEMBLY_USAGE_OCCURRENCE('Flat Washer - M5:3',
'Flat Washer - M5:3','Flat Washer - M5:3',#20407,#20415,
'Flat Washer - M5:3');
#428=NEXT_ASSEMBLY_USAGE_OCCURRENCE('Cap Screw - M5x20:3',
'Cap Screw - M5x20:3','Cap Screw - M5x20:3',#20407,#20416,
'Cap Screw - M5x20:3');
#429=NEXT_ASSEMBLY_USAGE_OCCURRENCE('Flat Washer - M5:4',
'Flat Washer - M5:4','Flat Washer - M5:4',#20407,#20415,
'Flat Washer - M5:4');
#430=NEXT_ASSEMBLY_USAGE_OCCURRENCE('Cap Screw - M5x20:4',
'Cap Screw - M5x20:4','Cap Screw - M5x20:4',#20407,#20416,
'Cap Screw - M5x20:4');
#431=NEXT_ASSEMBLY_USAGE_OCCURRENCE('Flat Washer - M5:5',
'Flat Washer - M5:5','Flat Washer - M5:5',#20407,#20415,
'Flat Washer - M5:5');
#432=NEXT_ASSEMBLY_USAGE_OCCURRENCE('Cap Screw - M5x20:5',
'Cap Screw - M5x20:5','Cap Screw - M5x20:5',#20407,#20416,
'Cap Screw - M5x20:5');
#433=NEXT_ASSEMBLY_USAGE_OCCURRENCE('M4x10 Cap Screw:18',
'M4x10 Cap Screw:18','M4x10 Cap Screw:18',#20407,#20417,
'M4x10 Cap Screw:18');
#434=NEXT_ASSEMBLY_USAGE_OCCURRENCE('M4x10 Cap Screw:19',
'M4x10 Cap Screw:19','M4x10 Cap Screw:19',#20407,#20417,
'M4x10 Cap Screw:19');
#435=NEXT_ASSEMBLY_USAGE_OCCURRENCE('Cap Screw - M4x16:16',
'Cap Screw - M4x16:16','Cap Screw - M4x16:16',#20407,#20418,
'Cap Screw - M4x16:16');
#436=NEXT_ASSEMBLY_USAGE_OCCURRENCE('Cap Screw - M4x16:17',
'Cap Screw - M4x16:17','Cap Screw - M4x16:17',#20407,#20418,
'Cap Screw - M4x16:17');
#437=NEXT_ASSEMBLY_USAGE_OCCURRENCE('Frame and belt envelope:1',
'Frame and belt envelope:1','Frame and belt envelope:1',#20366,#20367,
'Frame and belt envelope:1');
#438=NEXT_ASSEMBLY_USAGE_OCCURRENCE('Drive pulley and shaft:1',
'Drive pulley and shaft:1','Drive pulley and shaft:1',#20366,#20392,
'Drive pulley and shaft:1');
#439=NEXT_ASSEMBLY_USAGE_OCCURRENCE('Return pulley and shaft:1',
'Return pulley and shaft:1','Return pulley and shaft:1',#20366,#20399,
'Return pulley and shaft:1');
#440=NEXT_ASSEMBLY_USAGE_OCCURRENCE('Moving carriage:1',
'Moving carriage:1','Moving carriage:1',#20366,#20407,
'Moving carriage:1');
#441=B_SPLINE_CURVE_WITH_KNOTS('',3,(#17380,#17381,#17382,#17383,#17384,
#17385,#17386,#17387,#17388,#17389,#17390,#17391,#17392,#17393,#17394,#17395,
#17396,#17397,#17398,#17399,#17400,#17401),.UNSPECIFIED.,.F.,.F.,(4,2,2,
2,2,2,2,2,2,2,4),(0.0473477652366656,0.126350602536658,0.189525903804987,
0.252701205073317,0.313298422430275,0.373895639787233,0.434492857144191,
0.495090074501149,0.558265375769478,0.621440677037807,0.7004435143378),
 .UNSPECIFIED.);
#442=B_SPLINE_CURVE_WITH_KNOTS('',3,(#17405,#17406,#17407,#17408,#17409,
#17410,#17411,#17412,#17413,#17414,#17415,#17416,#17417,#17418,#17419,#17420,
#17421,#17422,#17423,#17424,#17425,#17426),.UNSPECIFIED.,.F.,.F.,(4,2,2,
2,2,2,2,2,2,2,4),(0.0464897534940957,0.0852567806515119,0.170513561303024,
0.246687263103517,0.308657850341199,0.370628437578881,0.432599024816563,
0.494569612054245,0.570743313854739,0.656000094506251,0.694767121663666),
 .UNSPECIFIED.);
#443=B_SPLINE_CURVE_WITH_KNOTS('',3,(#17432,#17433,#17434,#17435,#17436,
#17437,#17438,#17439,#17440,#17441,#17442,#17443,#17444,#17445,#17446,#17447,
#17448,#17449,#17450,#17451,#17452,#17453),.UNSPECIFIED.,.F.,.F.,(4,2,2,
2,2,2,2,2,2,2,4),(0.0464897534940957,0.0852567806515118,0.170513561303024,
0.246687263103517,0.308657850341199,0.370628437578881,0.432599024816563,
0.494569612054245,0.570743313854738,0.65600009450625,0.694767121663666),
 .UNSPECIFIED.);
#444=B_SPLINE_CURVE_WITH_KNOTS('',3,(#17457,#17458,#17459,#17460,#17461,
#17462,#17463,#17464,#17465,#17466,#17467,#17468,#17469,#17470,#17471,#17472,
#17473,#17474,#17475,#17476,#17477,#17478),.UNSPECIFIED.,.F.,.F.,(4,2,2,
2,2,2,2,2,2,2,4),(0.0464897534940957,0.0852567806515119,0.170513561303024,
0.246687263103517,0.308657850341199,0.370628437578881,0.432599024816563,
0.494569612054245,0.570743313854739,0.656000094506251,0.694767121663666),
 .UNSPECIFIED.);
#445=B_SPLINE_CURVE_WITH_KNOTS('',3,(#17482,#17483,#17484,#17485,#17486,
#17487,#17488,#17489,#17490,#17491,#17492,#17493),.UNSPECIFIED.,.F.,.F.,
(4,2,2,2,2,4),(0.0464897534940957,0.0852567806515119,0.170513561303024,
0.246687263103517,0.308657850341199,0.370628437578881),.UNSPECIFIED.);
#446=B_SPLINE_CURVE_WITH_KNOTS('',3,(#17498,#17499,#17500,#17501,#17502,
#17503,#17504,#17505,#17506,#17507,#17508,#17509),.UNSPECIFIED.,.F.,.F.,
(4,2,2,2,2,4),(0.370628437578881,0.432599024816563,0.494569612054245,0.570743313854738,
0.65600009450625,0.694767121663666),.UNSPECIFIED.);
#447=B_SPLINE_CURVE_WITH_KNOTS('',3,(#17513,#17514,#17515,#17516,#17517,
#17518,#17519,#17520,#17521,#17522,#17523,#17524,#17525,#17526,#17527,#17528,
#17529,#17530,#17531,#17532,#17533,#17534),.UNSPECIFIED.,.F.,.F.,(4,2,2,
2,2,2,2,2,2,2,4),(0.0464897534940957,0.0852567806515121,0.170513561303024,
0.246687263103518,0.308657850341199,0.370628437578881,0.432599024816563,
0.494569612054245,0.570743313854738,0.65600009450625,0.694767121663666),
 .UNSPECIFIED.);
#448=B_SPLINE_CURVE_WITH_KNOTS('',3,(#17538,#17539,#17540,#17541,#17542,
#17543,#17544,#17545,#17546,#17547,#17548,#17549,#17550,#17551,#17552,#17553,
#17554,#17555,#17556,#17557,#17558,#17559),.UNSPECIFIED.,.F.,.F.,(4,2,2,
2,2,2,2,2,2,2,4),(0.0464897534940957,0.0852567806515119,0.170513561303024,
0.246687263103517,0.308657850341199,0.370628437578881,0.432599024816563,
0.494569612054245,0.570743313854738,0.65600009450625,0.694767121663667),
 .UNSPECIFIED.);
#449=B_SPLINE_CURVE_WITH_KNOTS('',3,(#17563,#17564,#17565,#17566,#17567,
#17568,#17569,#17570,#17571,#17572,#17573,#17574,#17575,#17576,#17577,#17578,
#17579,#17580,#17581,#17582,#17583,#17584),.UNSPECIFIED.,.F.,.F.,(4,2,2,
2,2,2,2,2,2,2,4),(0.0464897534940957,0.0852567806515119,0.170513561303024,
0.246687263103517,0.308657850341199,0.370628437578881,0.432599024816563,
0.494569612054245,0.570743313854738,0.65600009450625,0.694767121663666),
 .UNSPECIFIED.);
#450=B_SPLINE_CURVE_WITH_KNOTS('',3,(#17588,#17589,#17590,#17591,#17592,
#17593,#17594,#17595,#17596,#17597,#17598,#17599,#17600,#17601,#17602,#17603,
#17604,#17605,#17606,#17607,#17608,#17609),.UNSPECIFIED.,.F.,.F.,(4,2,2,
2,2,2,2,2,2,2,4),(0.0464897534940957,0.0852567806515119,0.170513561303024,
0.246687263103517,0.308657850341199,0.370628437578881,0.432599024816563,
0.494569612054245,0.570743313854739,0.656000094506251,0.694767121663667),
 .UNSPECIFIED.);
#451=B_SPLINE_CURVE_WITH_KNOTS('',3,(#17617,#17618,#17619,#17620,#17621,
#17622,#17623,#17624,#17625,#17626,#17627,#17628,#17629,#17630,#17631,#17632,
#17633,#17634,#17635,#17636,#17637,#17638),.UNSPECIFIED.,.F.,.F.,(4,2,2,
2,2,2,2,2,2,2,4),(0.0473477652366656,0.126350602536658,0.189525903804987,
0.252701205073316,0.313298422430274,0.373895639787232,0.434492857144191,
0.495090074501149,0.558265375769478,0.621440677037807,0.7004435143378),
 .UNSPECIFIED.);
#452=B_SPLINE_CURVE_WITH_KNOTS('',3,(#17646,#17647,#17648,#17649,#17650,
#17651,#17652,#17653,#17654,#17655,#17656,#17657,#17658,#17659,#17660,#17661,
#17662,#17663,#17664,#17665,#17666,#17667),.UNSPECIFIED.,.F.,.F.,(4,2,2,
2,2,2,2,2,2,2,4),(0.0473477652366656,0.126350602536658,0.189525903804987,
0.252701205073317,0.313298422430275,0.373895639787233,0.434492857144191,
0.495090074501149,0.558265375769478,0.621440677037807,0.7004435143378),
 .UNSPECIFIED.);
#453=B_SPLINE_CURVE_WITH_KNOTS('',3,(#17676,#17677,#17678,#17679,#17680,
#17681,#17682,#17683,#17684,#17685,#17686,#17687),.UNSPECIFIED.,.F.,.F.,
(4,2,2,2,2,4),(0.0473477652366656,0.126350602536658,0.189525903804987,0.252701205073316,
0.313298422430275,0.373895639787233),.UNSPECIFIED.);
#454=B_SPLINE_CURVE_WITH_KNOTS('',3,(#17689,#17690,#17691,#17692,#17693,
#17694,#17695,#17696,#17697,#17698,#17699,#17700),.UNSPECIFIED.,.F.,.F.,
(4,2,2,2,2,4),(0.373895639787233,0.434492857144191,0.495090074501149,0.558265375769478,
0.621440677037807,0.7004435143378),.UNSPECIFIED.);
#455=B_SPLINE_CURVE_WITH_KNOTS('',3,(#17707,#17708,#17709,#17710,#17711,
#17712,#17713,#17714,#17715,#17716,#17717,#17718,#17719,#17720,#17721,#17722,
#17723,#17724,#17725,#17726,#17727,#17728),.UNSPECIFIED.,.F.,.F.,(4,2,2,
2,2,2,2,2,2,2,4),(0.0473477652366656,0.126350602536658,0.189525903804987,
0.252701205073316,0.313298422430275,0.373895639787233,0.434492857144191,
0.495090074501149,0.558265375769478,0.621440677037807,0.7004435143378),
 .UNSPECIFIED.);
#456=B_SPLINE_CURVE_WITH_KNOTS('',3,(#17736,#17737,#17738,#17739,#17740,
#17741,#17742,#17743,#17744,#17745,#17746,#17747,#17748,#17749,#17750,#17751,
#17752,#17753,#17754,#17755,#17756,#17757),.UNSPECIFIED.,.F.,.F.,(4,2,2,
2,2,2,2,2,2,2,4),(0.0473477652366656,0.126350602536658,0.189525903804987,
0.252701205073317,0.313298422430275,0.373895639787233,0.434492857144191,
0.495090074501149,0.558265375769478,0.621440677037807,0.7004435143378),
 .UNSPECIFIED.);
#457=B_SPLINE_CURVE_WITH_KNOTS('',3,(#17765,#17766,#17767,#17768,#17769,
#17770,#17771,#17772,#17773,#17774,#17775,#17776,#17777,#17778,#17779,#17780,
#17781,#17782,#17783,#17784,#17785,#17786),.UNSPECIFIED.,.F.,.F.,(4,2,2,
2,2,2,2,2,2,2,4),(0.0473477652366656,0.126350602536658,0.189525903804987,
0.252701205073316,0.313298422430275,0.373895639787233,0.434492857144191,
0.495090074501149,0.558265375769478,0.621440677037807,0.7004435143378),
 .UNSPECIFIED.);
#458=B_SPLINE_CURVE_WITH_KNOTS('',3,(#17795,#17796,#17797,#17798,#17799,
#17800,#17801,#17802,#17803,#17804,#17805,#17806,#17807,#17808,#17809,#17810,
#17811,#17812,#17813,#17814,#17815,#17816),.UNSPECIFIED.,.F.,.F.,(4,2,2,
2,2,2,2,2,2,2,4),(0.0473477652366656,0.126350602536658,0.189525903804987,
0.252701205073317,0.313298422430275,0.373895639787233,0.434492857144191,
0.495090074501149,0.558265375769478,0.621440677037807,0.7004435143378),
 .UNSPECIFIED.);
#459=B_SPLINE_CURVE_WITH_KNOTS('',3,(#18624,#18625,#18626,#18627,#18628,
#18629,#18630,#18631,#18632,#18633),.UNSPECIFIED.,.F.,.F.,(4,2,2,2,4),(0.566550474129931,
0.613761886174531,0.66097329821913,0.708186965196186,0.755400632173242),
 .UNSPECIFIED.);
#460=B_SPLINE_CURVE_WITH_KNOTS('',3,(#18635,#18636,#18637,#18638,#18639,
#18640,#18641,#18642,#18643,#18644,#18645,#18646,#18647,#18648,#18649,#18650,
#18651,#18652),.UNSPECIFIED.,.F.,.F.,(4,2,2,2,2,2,2,2,4),(0.18885015804331,
0.23606157008791,0.283272982132509,0.330486649109565,0.377700316086621,
0.424913983063677,0.472127650040732,0.519339062085332,0.566550474129931),
 .UNSPECIFIED.);
#461=B_SPLINE_CURVE_WITH_KNOTS('',3,(#18653,#18654,#18655,#18656,#18657,
#18658,#18659,#18660,#18661,#18662),.UNSPECIFIED.,.F.,.F.,(4,2,2,2,4),(0.755400632173242,
0.802614299150298,0.849827966127353,0.897039378171953,0.944250790216552),
 .UNSPECIFIED.);
#462=B_SPLINE_CURVE_WITH_KNOTS('',3,(#18666,#18667,#18668,#18669,#18670,
#18671,#18672,#18673,#18674,#18675),.UNSPECIFIED.,.F.,.F.,(4,2,2,2,4),(0.189723673274825,
0.237146208024627,0.28456874277443,0.33200804466204,0.37944734654965),
 .UNSPECIFIED.);
#463=B_SPLINE_CURVE_WITH_KNOTS('',3,(#18677,#18678,#18679,#18680,#18681,
#18682,#18683,#18684,#18685,#18686),.UNSPECIFIED.,.F.,.F.,(4,2,2,2,4),(0.,
0.0474393018876097,0.0948786037752193,0.142301138525022,0.189723673274825),
 .UNSPECIFIED.);
#464=B_SPLINE_CURVE_WITH_KNOTS('',3,(#18688,#18689,#18690,#18691,#18692,
#18693,#18694,#18695,#18696,#18697),.UNSPECIFIED.,.F.,.F.,(4,2,2,2,4),(0.569171019824474,
0.616593554574277,0.66401608932408,0.711455391211689,0.758894693099299),
 .UNSPECIFIED.);
#465=B_SPLINE_CURVE_WITH_KNOTS('',3,(#18698,#18699,#18700,#18701,#18702,
#18703,#18704,#18705,#18706,#18707),.UNSPECIFIED.,.F.,.F.,(4,2,2,2,4),(0.37944734654965,
0.426886648437259,0.474325950324869,0.521748485074671,0.569171019824474),
 .UNSPECIFIED.);
#466=B_SPLINE_CURVE_WITH_KNOTS('',3,(#18711,#18712,#18713,#18714,#18715,
#18716,#18717,#18718,#18719,#18720,#18721,#18722,#18723,#18724,#18725,#18726,
#18727,#18728),.UNSPECIFIED.,.F.,.F.,(4,2,2,2,2,2,2,2,4),(0.,0.0474393018876097,
0.0948786037752194,0.142301138525022,0.189723673274825,0.237146208024628,
0.28456874277443,0.33200804466204,0.37944734654965),.UNSPECIFIED.);
#467=B_SPLINE_CURVE_WITH_KNOTS('',3,(#18729,#18730,#18731,#18732,#18733,
#18734,#18735,#18736,#18737,#18738,#18739,#18740,#18741,#18742,#18743,#18744,
#18745,#18746),.UNSPECIFIED.,.F.,.F.,(4,2,2,2,2,2,2,2,4),(0.37944734654965,
0.426886648437259,0.474325950324869,0.521748485074672,0.569171019824474,
0.616593554574277,0.66401608932408,0.711455391211689,0.758894693099299),
 .UNSPECIFIED.);
#468=B_SPLINE_CURVE_WITH_KNOTS('',3,(#18750,#18751,#18752,#18753,#18754,
#18755,#18756,#18757,#18758,#18759),.UNSPECIFIED.,.F.,.F.,(4,2,2,2,4),(0.566550474129931,
0.613761886174531,0.66097329821913,0.708186965196186,0.755400632173242),
 .UNSPECIFIED.);
#469=B_SPLINE_CURVE_WITH_KNOTS('',3,(#18761,#18762,#18763,#18764,#18765,
#18766,#18767,#18768,#18769,#18770,#18771,#18772,#18773,#18774,#18775,#18776,
#18777,#18778),.UNSPECIFIED.,.F.,.F.,(4,2,2,2,2,2,2,2,4),(0.188850158043311,
0.23606157008791,0.283272982132509,0.330486649109565,0.377700316086621,
0.424913983063677,0.472127650040733,0.519339062085332,0.566550474129931),
 .UNSPECIFIED.);
#470=B_SPLINE_CURVE_WITH_KNOTS('',3,(#18779,#18780,#18781,#18782,#18783,
#18784,#18785,#18786,#18787,#18788),.UNSPECIFIED.,.F.,.F.,(4,2,2,2,4),(0.755400632173242,
0.802614299150298,0.849827966127354,0.897039378171953,0.944250790216552),
 .UNSPECIFIED.);
#471=B_SPLINE_CURVE_WITH_KNOTS('',3,(#18798,#18799,#18800,#18801,#18802,
#18803,#18804,#18805,#18806,#18807,#18808,#18809,#18810,#18811,#18812,#18813,
#18814,#18815),.UNSPECIFIED.,.F.,.F.,(4,2,2,2,2,2,2,2,4),(0.18885015804331,
0.23606157008791,0.283272982132509,0.330486649109565,0.377700316086621,
0.424913983063677,0.472127650040732,0.519339062085332,0.566550474129931),
 .UNSPECIFIED.);
#472=B_SPLINE_CURVE_WITH_KNOTS('',3,(#18817,#18818,#18819,#18820,#18821,
#18822,#18823,#18824,#18825,#18826),.UNSPECIFIED.,.F.,.F.,(4,2,2,2,4),(0.566550474129931,
0.613761886174531,0.66097329821913,0.708186965196186,0.755400632173242),
 .UNSPECIFIED.);
#473=B_SPLINE_CURVE_WITH_KNOTS('',3,(#18827,#18828,#18829,#18830,#18831,
#18832,#18833,#18834,#18835,#18836),.UNSPECIFIED.,.F.,.F.,(4,2,2,2,4),(0.755400632173242,
0.802614299150298,0.849827966127353,0.897039378171953,0.944250790216552),
 .UNSPECIFIED.);
#474=B_SPLINE_CURVE_WITH_KNOTS('',3,(#18839,#18840,#18841,#18842,#18843,
#18844,#18845,#18846,#18847,#18848,#18849,#18850,#18851,#18852,#18853,#18854,
#18855,#18856),.UNSPECIFIED.,.F.,.F.,(4,2,2,2,2,2,2,2,4),(0.188850158043311,
0.23606157008791,0.283272982132509,0.330486649109565,0.377700316086621,
0.424913983063677,0.472127650040733,0.519339062085332,0.566550474129932),
 .UNSPECIFIED.);
#475=B_SPLINE_CURVE_WITH_KNOTS('',3,(#18858,#18859,#18860,#18861,#18862,
#18863,#18864,#18865,#18866,#18867),.UNSPECIFIED.,.F.,.F.,(4,2,2,2,4),(0.566550474129932,
0.613761886174531,0.66097329821913,0.708186965196186,0.755400632173242),
 .UNSPECIFIED.);
#476=B_SPLINE_CURVE_WITH_KNOTS('',3,(#18868,#18869,#18870,#18871,#18872,
#18873,#18874,#18875,#18876,#18877),.UNSPECIFIED.,.F.,.F.,(4,2,2,2,4),(0.755400632173242,
0.802614299150298,0.849827966127354,0.897039378171953,0.944250790216552),
 .UNSPECIFIED.);
#477=B_SPLINE_CURVE_WITH_KNOTS('',3,(#18882,#18883,#18884,#18885,#18886,
#18887,#18888,#18889,#18890,#18891,#18892,#18893,#18894,#18895,#18896,#18897,
#18898,#18899),.UNSPECIFIED.,.F.,.F.,(4,2,2,2,2,2,2,2,4),(0.,0.0474393018876097,
0.0948786037752193,0.142301138525022,0.189723673274825,0.237146208024627,
0.28456874277443,0.33200804466204,0.37944734654965),.UNSPECIFIED.);
#478=B_SPLINE_CURVE_WITH_KNOTS('',3,(#18900,#18901,#18902,#18903,#18904,
#18905,#18906,#18907,#18908,#18909,#18910,#18911,#18912,#18913,#18914,#18915,
#18916,#18917),.UNSPECIFIED.,.F.,.F.,(4,2,2,2,2,2,2,2,4),(0.37944734654965,
0.426886648437259,0.474325950324869,0.521748485074672,0.569171019824474,
0.616593554574277,0.66401608932408,0.711455391211689,0.758894693099299),
 .UNSPECIFIED.);
#479=B_SPLINE_CURVE_WITH_KNOTS('',3,(#18921,#18922,#18923,#18924,#18925,
#18926,#18927,#18928,#18929,#18930,#18931,#18932,#18933,#18934,#18935,#18936,
#18937,#18938),.UNSPECIFIED.,.F.,.F.,(4,2,2,2,2,2,2,2,4),(0.,0.0474393018876097,
0.0948786037752194,0.142301138525022,0.189723673274825,0.237146208024627,
0.28456874277443,0.33200804466204,0.37944734654965),.UNSPECIFIED.);
#480=B_SPLINE_CURVE_WITH_KNOTS('',3,(#18939,#18940,#18941,#18942,#18943,
#18944,#18945,#18946,#18947,#18948,#18949,#18950,#18951,#18952,#18953,#18954,
#18955,#18956),.UNSPECIFIED.,.F.,.F.,(4,2,2,2,2,2,2,2,4),(0.37944734654965,
0.426886648437259,0.474325950324869,0.521748485074672,0.569171019824474,
0.616593554574277,0.66401608932408,0.711455391211689,0.758894693099299),
 .UNSPECIFIED.);
#481=SPHERICAL_SURFACE('',#11958,0.23815);
#482=SPHERICAL_SURFACE('',#11960,0.23815);
#483=SPHERICAL_SURFACE('',#11962,0.23815);
#484=SPHERICAL_SURFACE('',#11964,0.23815);
#485=SPHERICAL_SURFACE('',#11966,0.23815);
#486=SPHERICAL_SURFACE('',#11968,0.23815);
#487=SPHERICAL_SURFACE('',#11970,0.23815);
#488=SPHERICAL_SURFACE('',#11972,0.23815);
#489=SPHERICAL_SURFACE('',#11975,0.247676);
#490=SPHERICAL_SURFACE('',#11991,0.247676);
#491=SPHERICAL_SURFACE('',#11996,0.247676);
#492=SPHERICAL_SURFACE('',#12001,0.247676);
#493=SPHERICAL_SURFACE('',#12006,0.247676);
#494=SPHERICAL_SURFACE('',#12011,0.247676);
#495=SPHERICAL_SURFACE('',#12016,0.247676);
#496=SPHERICAL_SURFACE('',#12024,0.247676);
#497=CONICAL_SURFACE('',#11929,0.53,0.785398163397448);
#498=CONICAL_SURFACE('',#11936,0.53,0.785398163397448);
#499=CONICAL_SURFACE('',#11949,1.47,0.785398163397449);
#500=CONICAL_SURFACE('',#11953,1.47,0.785398163397449);
#501=CONICAL_SURFACE('',#12134,0.4,0.785398163397448);
#502=CONICAL_SURFACE('',#12138,0.41,0.785398163397448);
#503=CONICAL_SURFACE('',#12142,0.26,0.463647609000806);
#504=CONICAL_SURFACE('',#12602,0.275,0.785398163397449);
#505=CONICAL_SURFACE('',#12615,0.4,0.785398163397448);
#506=CONICAL_SURFACE('',#12619,0.41,0.785398163397448);
#507=CONICAL_SURFACE('',#12623,0.26,0.463647609000806);
#508=CONICAL_SURFACE('',#12627,0.225,0.785398163397448);
#509=CONICAL_SURFACE('',#12651,0.325,0.785398163397448);
#510=CONICAL_SURFACE('',#12655,0.335,0.785398163397448);
#511=CONICAL_SURFACE('',#12659,0.21,0.463647609000806);
#512=CONICAL_SURFACE('',#12665,0.325,0.785398163397448);
#513=CONICAL_SURFACE('',#12669,0.335,0.785398163397448);
#514=CONICAL_SURFACE('',#12673,0.21,0.463647609000806);
#515=CONICAL_SURFACE('',#12677,0.18,0.785398163397448);
#516=TOROIDAL_SURFACE('',#11918,1.,0.247676);
#517=TOROIDAL_SURFACE('',#11938,1.,0.247676);
#518=SHAPE_REPRESENTATION_RELATIONSHIP('SRR','None',#20314,#564);
#519=SHAPE_REPRESENTATION_RELATIONSHIP('SRR','None',#20315,#565);
#520=SHAPE_REPRESENTATION_RELATIONSHIP('SRR','None',#20316,#566);
#521=SHAPE_REPRESENTATION_RELATIONSHIP('SRR','None',#20317,#567);
#522=SHAPE_REPRESENTATION_RELATIONSHIP('SRR','None',#20318,#568);
#523=SHAPE_REPRESENTATION_RELATIONSHIP('SRR','None',#20319,#569);
#524=SHAPE_REPRESENTATION_RELATIONSHIP('SRR','None',#20320,#570);
#525=SHAPE_REPRESENTATION_RELATIONSHIP('SRR','None',#20321,#571);
#526=SHAPE_REPRESENTATION_RELATIONSHIP('SRR','None',#20322,#572);
#527=SHAPE_REPRESENTATION_RELATIONSHIP('SRR','None',#20323,#573);
#528=SHAPE_REPRESENTATION_RELATIONSHIP('SRR','None',#20324,#574);
#529=SHAPE_REPRESENTATION_RELATIONSHIP('SRR','None',#20325,#575);
#530=SHAPE_REPRESENTATION_RELATIONSHIP('SRR','None',#20326,#576);
#531=SHAPE_REPRESENTATION_RELATIONSHIP('SRR','None',#20327,#577);
#532=SHAPE_REPRESENTATION_RELATIONSHIP('SRR','None',#20329,#578);
#533=SHAPE_REPRESENTATION_RELATIONSHIP('SRR','None',#20330,#579);
#534=SHAPE_REPRESENTATION_RELATIONSHIP('SRR','None',#20331,#580);
#535=SHAPE_REPRESENTATION_RELATIONSHIP('SRR','None',#20332,#581);
#536=SHAPE_REPRESENTATION_RELATIONSHIP('SRR','None',#20333,#582);
#537=SHAPE_REPRESENTATION_RELATIONSHIP('SRR','None',#20334,#583);
#538=SHAPE_REPRESENTATION_RELATIONSHIP('SRR','None',#20335,#584);
#539=SHAPE_REPRESENTATION_RELATIONSHIP('SRR','None',#20336,#585);
#540=SHAPE_REPRESENTATION_RELATIONSHIP('SRR','None',#20337,#586);
#541=SHAPE_REPRESENTATION_RELATIONSHIP('SRR','None',#20339,#587);
#542=SHAPE_REPRESENTATION_RELATIONSHIP('SRR','None',#20340,#588);
#543=SHAPE_REPRESENTATION_RELATIONSHIP('SRR','None',#20341,#589);
#544=SHAPE_REPRESENTATION_RELATIONSHIP('SRR','None',#20342,#590);
#545=SHAPE_REPRESENTATION_RELATIONSHIP('SRR','None',#20343,#591);
#546=SHAPE_REPRESENTATION_RELATIONSHIP('SRR','None',#20344,#592);
#547=SHAPE_REPRESENTATION_RELATIONSHIP('SRR','None',#20346,#593);
#548=SHAPE_REPRESENTATION_RELATIONSHIP('SRR','None',#20347,#594);
#549=SHAPE_REPRESENTATION_RELATIONSHIP('SRR','None',#20348,#595);
#550=SHAPE_REPRESENTATION_RELATIONSHIP('SRR','None',#20349,#596);
#551=SHAPE_REPRESENTATION_RELATIONSHIP('SRR','None',#20350,#597);
#552=SHAPE_REPRESENTATION_RELATIONSHIP('SRR','None',#20351,#598);
#553=SHAPE_REPRESENTATION_RELATIONSHIP('SRR','None',#20352,#599);
#554=SHAPE_REPRESENTATION_RELATIONSHIP('SRR','None',#20354,#600);
#555=SHAPE_REPRESENTATION_RELATIONSHIP('SRR','None',#20355,#601);
#556=SHAPE_REPRESENTATION_RELATIONSHIP('SRR','None',#20356,#602);
#557=SHAPE_REPRESENTATION_RELATIONSHIP('SRR','None',#20358,#603);
#558=SHAPE_REPRESENTATION_RELATIONSHIP('SRR','None',#20359,#604);
#559=SHAPE_REPRESENTATION_RELATIONSHIP('SRR','None',#20360,#605);
#560=SHAPE_REPRESENTATION_RELATIONSHIP('SRR','None',#20361,#606);
#561=SHAPE_REPRESENTATION_RELATIONSHIP('SRR','None',#20362,#607);
#562=SHAPE_REPRESENTATION_RELATIONSHIP('SRR','None',#20363,#608);
#563=SHAPE_REPRESENTATION_RELATIONSHIP('SRR','None',#20364,#609);
#564=ADVANCED_BREP_SHAPE_REPRESENTATION('',(#666),#20045);
#565=ADVANCED_BREP_SHAPE_REPRESENTATION('',(#667,#668),#20046);
#566=ADVANCED_BREP_SHAPE_REPRESENTATION('',(#669,#670),#20047);
#567=ADVANCED_BREP_SHAPE_REPRESENTATION('',(#671),#20048);
#568=ADVANCED_BREP_SHAPE_REPRESENTATION('',(#672),#20049);
#569=ADVANCED_BREP_SHAPE_REPRESENTATION('',(#673),#20050);
#570=ADVANCED_BREP_SHAPE_REPRESENTATION('',(#674),#20051);
#571=ADVANCED_BREP_SHAPE_REPRESENTATION('',(#675),#20052);
#572=ADVANCED_BREP_SHAPE_REPRESENTATION('',(#676),#20053);
#573=ADVANCED_BREP_SHAPE_REPRESENTATION('',(#677),#20054);
#574=ADVANCED_BREP_SHAPE_REPRESENTATION('',(#678),#20055);
#575=ADVANCED_BREP_SHAPE_REPRESENTATION('',(#679),#20056);
#576=ADVANCED_BREP_SHAPE_REPRESENTATION('',(#680),#20057);
#577=ADVANCED_BREP_SHAPE_REPRESENTATION('',(#681),#20058);
#578=ADVANCED_BREP_SHAPE_REPRESENTATION('',(#682),#20060);
#579=ADVANCED_BREP_SHAPE_REPRESENTATION('',(#683),#20061);
#580=ADVANCED_BREP_SHAPE_REPRESENTATION('',(#684,#685,#686,#687,#688,#689,
#690,#691),#20062);
#581=ADVANCED_BREP_SHAPE_REPRESENTATION('',(#692),#20063);
#582=ADVANCED_BREP_SHAPE_REPRESENTATION('',(#693,#694),#20064);
#583=ADVANCED_BREP_SHAPE_REPRESENTATION('',(#695),#20065);
#584=ADVANCED_BREP_SHAPE_REPRESENTATION('',(#696),#20066);
#585=ADVANCED_BREP_SHAPE_REPRESENTATION('',(#15),#20067);
#586=ADVANCED_BREP_SHAPE_REPRESENTATION('',(#697),#20068);
#587=ADVANCED_BREP_SHAPE_REPRESENTATION('',(#698),#20070);
#588=ADVANCED_BREP_SHAPE_REPRESENTATION('',(#699),#20071);
#589=ADVANCED_BREP_SHAPE_REPRESENTATION('',(#700),#20072);
#590=ADVANCED_BREP_SHAPE_REPRESENTATION('',(#701),#20073);
#591=ADVANCED_BREP_SHAPE_REPRESENTATION('',(#702),#20074);
#592=ADVANCED_BREP_SHAPE_REPRESENTATION('',(#703),#20075);
#593=ADVANCED_BREP_SHAPE_REPRESENTATION('',(#704),#20077);
#594=ADVANCED_BREP_SHAPE_REPRESENTATION('',(#705),#20078);
#595=ADVANCED_BREP_SHAPE_REPRESENTATION('',(#706),#20079);
#596=ADVANCED_BREP_SHAPE_REPRESENTATION('',(#707),#20080);
#597=ADVANCED_BREP_SHAPE_REPRESENTATION('',(#708),#20081);
#598=ADVANCED_BREP_SHAPE_REPRESENTATION('',(#709),#20082);
#599=ADVANCED_BREP_SHAPE_REPRESENTATION('',(#710),#20083);
#600=ADVANCED_BREP_SHAPE_REPRESENTATION('',(#711),#20085);
#601=ADVANCED_BREP_SHAPE_REPRESENTATION('',(#712),#20086);
#602=ADVANCED_BREP_SHAPE_REPRESENTATION('',(#713),#20087);
#603=ADVANCED_BREP_SHAPE_REPRESENTATION('',(#714),#20089);
#604=ADVANCED_BREP_SHAPE_REPRESENTATION('',(#715),#20090);
#605=ADVANCED_BREP_SHAPE_REPRESENTATION('',(#716),#20091);
#606=ADVANCED_BREP_SHAPE_REPRESENTATION('',(#717),#20092);
#607=ADVANCED_BREP_SHAPE_REPRESENTATION('',(#16),#20093);
#608=ADVANCED_BREP_SHAPE_REPRESENTATION('',(#17),#20094);
#609=ADVANCED_BREP_SHAPE_REPRESENTATION('',(#18),#20095);
#610=STYLED_ITEM('',(#20629),#666);
#611=STYLED_ITEM('',(#20664),#667);
#612=STYLED_ITEM('',(#20664),#668);
#613=STYLED_ITEM('',(#20664),#669);
#614=STYLED_ITEM('',(#20664),#670);
#615=STYLED_ITEM('',(#20650),#671);
#616=STYLED_ITEM('',(#20643),#672);
#617=STYLED_ITEM('',(#20650),#673);
#618=STYLED_ITEM('',(#20650),#674);
#619=STYLED_ITEM('',(#20650),#675);
#620=STYLED_ITEM('',(#20643),#676);
#621=STYLED_ITEM('',(#20650),#677);
#622=STYLED_ITEM('',(#20650),#678);
#623=STYLED_ITEM('',(#20657),#679);
#624=STYLED_ITEM('',(#20636),#680);
#625=STYLED_ITEM('',(#20636),#681);
#626=STYLED_ITEM('',(#20650),#682);
#627=STYLED_ITEM('',(#20650),#683);
#628=STYLED_ITEM('',(#20650),#684);
#629=STYLED_ITEM('',(#20650),#685);
#630=STYLED_ITEM('',(#20650),#686);
#631=STYLED_ITEM('',(#20650),#687);
#632=STYLED_ITEM('',(#20650),#688);
#633=STYLED_ITEM('',(#20650),#689);
#634=STYLED_ITEM('',(#20650),#690);
#635=STYLED_ITEM('',(#20650),#691);
#636=STYLED_ITEM('',(#20650),#692);
#637=STYLED_ITEM('',(#20650),#693);
#638=STYLED_ITEM('',(#20650),#694);
#639=STYLED_ITEM('',(#20636),#695);
#640=STYLED_ITEM('',(#20657),#696);
#641=STYLED_ITEM('',(#20657),#15);
#642=STYLED_ITEM('',(#20643),#697);
#643=STYLED_ITEM('',(#20650),#698);
#644=STYLED_ITEM('',(#20664),#699);
#645=STYLED_ITEM('',(#20636),#700);
#646=STYLED_ITEM('',(#20657),#701);
#647=STYLED_ITEM('',(#20657),#702);
#648=STYLED_ITEM('',(#20643),#703);
#649=STYLED_ITEM('',(#20650),#704);
#650=STYLED_ITEM('',(#20664),#705);
#651=STYLED_ITEM('',(#20636),#706);
#652=STYLED_ITEM('',(#20657),#707);
#653=STYLED_ITEM('',(#20657),#708);
#654=STYLED_ITEM('',(#20643),#709);
#655=STYLED_ITEM('',(#20664),#710);
#656=STYLED_ITEM('',(#20643),#711);
#657=STYLED_ITEM('',(#20657),#712);
#658=STYLED_ITEM('',(#20657),#713);
#659=STYLED_ITEM('',(#20629),#714);
#660=STYLED_ITEM('',(#20643),#715);
#661=STYLED_ITEM('',(#20664),#716);
#662=STYLED_ITEM('',(#20657),#717);
#663=STYLED_ITEM('',(#20657),#16);
#664=STYLED_ITEM('',(#20657),#17);
#665=STYLED_ITEM('',(#20657),#18);
#666=MANIFOLD_SOLID_BREP('Body1',#10923);
#667=MANIFOLD_SOLID_BREP('Body1',#10924);
#668=MANIFOLD_SOLID_BREP('Body2',#10925);
#669=MANIFOLD_SOLID_BREP('Body1',#10926);
#670=MANIFOLD_SOLID_BREP('Body2',#10927);
#671=MANIFOLD_SOLID_BREP('Body1',#10928);
#672=MANIFOLD_SOLID_BREP('Body1',#10929);
#673=MANIFOLD_SOLID_BREP('Body1',#10930);
#674=MANIFOLD_SOLID_BREP('Body1',#10931);
#675=MANIFOLD_SOLID_BREP('Body1',#10932);
#676=MANIFOLD_SOLID_BREP('Body1',#10933);
#677=MANIFOLD_SOLID_BREP('Body1',#10934);
#678=MANIFOLD_SOLID_BREP('Body1',#10935);
#679=MANIFOLD_SOLID_BREP('Body1',#10936);
#680=MANIFOLD_SOLID_BREP('Body1',#10937);
#681=MANIFOLD_SOLID_BREP('Body1',#10938);
#682=MANIFOLD_SOLID_BREP('Body1',#10939);
#683=MANIFOLD_SOLID_BREP('Body1',#10940);
#684=MANIFOLD_SOLID_BREP('Body1',#10941);
#685=MANIFOLD_SOLID_BREP('Body2',#10942);
#686=MANIFOLD_SOLID_BREP('Body3',#10943);
#687=MANIFOLD_SOLID_BREP('Body4',#10944);
#688=MANIFOLD_SOLID_BREP('Body5',#10945);
#689=MANIFOLD_SOLID_BREP('Body6',#10946);
#690=MANIFOLD_SOLID_BREP('Body7',#10947);
#691=MANIFOLD_SOLID_BREP('Body8',#10948);
#692=MANIFOLD_SOLID_BREP('Continuous crown cage',#10949);
#693=MANIFOLD_SOLID_BREP('Body1',#10950);
#694=MANIFOLD_SOLID_BREP('Body2',#10951);
#695=MANIFOLD_SOLID_BREP('Body1',#10952);
#696=MANIFOLD_SOLID_BREP('Body1',#10953);
#697=MANIFOLD_SOLID_BREP('Body1',#10956);
#698=MANIFOLD_SOLID_BREP('Body1',#10957);
#699=MANIFOLD_SOLID_BREP('Body1',#10958);
#700=MANIFOLD_SOLID_BREP('Body1',#10959);
#701=MANIFOLD_SOLID_BREP('Body1',#10960);
#702=MANIFOLD_SOLID_BREP('Body1',#10961);
#703=MANIFOLD_SOLID_BREP('Body1',#10962);
#704=MANIFOLD_SOLID_BREP('Body1',#10963);
#705=MANIFOLD_SOLID_BREP('Body1',#10964);
#706=MANIFOLD_SOLID_BREP('Body1',#10965);
#707=MANIFOLD_SOLID_BREP('Body1',#10966);
#708=MANIFOLD_SOLID_BREP('Body1',#10967);
#709=MANIFOLD_SOLID_BREP('Body1',#10968);
#710=MANIFOLD_SOLID_BREP('Body1',#10969);
#711=MANIFOLD_SOLID_BREP('Body1',#10970);
#712=MANIFOLD_SOLID_BREP('Body1',#10971);
#713=MANIFOLD_SOLID_BREP('Body1',#10972);
#714=MANIFOLD_SOLID_BREP('Body1',#10973);
#715=MANIFOLD_SOLID_BREP('Body1',#10974);
#716=MANIFOLD_SOLID_BREP('Body1',#10975);
#717=MANIFOLD_SOLID_BREP('Body1',#10976);
#718=FACE_BOUND('',#1913,.T.);
#719=FACE_BOUND('',#1914,.T.);
#720=FACE_BOUND('',#1915,.T.);
#721=FACE_BOUND('',#1916,.T.);
#722=FACE_BOUND('',#1917,.T.);
#723=FACE_BOUND('',#1918,.T.);
#724=FACE_BOUND('',#1919,.T.);
#725=FACE_BOUND('',#1920,.T.);
#726=FACE_BOUND('',#1921,.T.);
#727=FACE_BOUND('',#1922,.T.);
#728=FACE_BOUND('',#1923,.T.);
#729=FACE_BOUND('',#1924,.T.);
#730=FACE_BOUND('',#1925,.T.);
#731=FACE_BOUND('',#1926,.T.);
#732=FACE_BOUND('',#1927,.T.);
#733=FACE_BOUND('',#1928,.T.);
#734=FACE_BOUND('',#1929,.T.);
#735=FACE_BOUND('',#1930,.T.);
#736=FACE_BOUND('',#1931,.T.);
#737=FACE_BOUND('',#1932,.T.);
#738=FACE_BOUND('',#1934,.T.);
#739=FACE_BOUND('',#1935,.T.);
#740=FACE_BOUND('',#1936,.T.);
#741=FACE_BOUND('',#1937,.T.);
#742=FACE_BOUND('',#1972,.T.);
#743=FACE_BOUND('',#1973,.T.);
#744=FACE_BOUND('',#1975,.T.);
#745=FACE_BOUND('',#1976,.T.);
#746=FACE_BOUND('',#1980,.T.);
#747=FACE_BOUND('',#1981,.T.);
#748=FACE_BOUND('',#1982,.T.);
#749=FACE_BOUND('',#1983,.T.);
#750=FACE_BOUND('',#1984,.T.);
#751=FACE_BOUND('',#1987,.T.);
#752=FACE_BOUND('',#1988,.T.);
#753=FACE_BOUND('',#1989,.T.);
#754=FACE_BOUND('',#1990,.T.);
#755=FACE_BOUND('',#1991,.T.);
#756=FACE_BOUND('',#1995,.T.);
#757=FACE_BOUND('',#1996,.T.);
#758=FACE_BOUND('',#1997,.T.);
#759=FACE_BOUND('',#1998,.T.);
#760=FACE_BOUND('',#2002,.T.);
#761=FACE_BOUND('',#2004,.T.);
#762=FACE_BOUND('',#2010,.T.);
#763=FACE_BOUND('',#2017,.T.);
#764=FACE_BOUND('',#2020,.T.);
#765=FACE_BOUND('',#2026,.T.);
#766=FACE_BOUND('',#2033,.T.);
#767=FACE_BOUND('',#2036,.T.);
#768=FACE_BOUND('',#2047,.T.);
#769=FACE_BOUND('',#2048,.T.);
#770=FACE_BOUND('',#2050,.T.);
#771=FACE_BOUND('',#2051,.T.);
#772=FACE_BOUND('',#2055,.T.);
#773=FACE_BOUND('',#2056,.T.);
#774=FACE_BOUND('',#2057,.T.);
#775=FACE_BOUND('',#2058,.T.);
#776=FACE_BOUND('',#2059,.T.);
#777=FACE_BOUND('',#2062,.T.);
#778=FACE_BOUND('',#2063,.T.);
#779=FACE_BOUND('',#2064,.T.);
#780=FACE_BOUND('',#2065,.T.);
#781=FACE_BOUND('',#2066,.T.);
#782=FACE_BOUND('',#2070,.T.);
#783=FACE_BOUND('',#2071,.T.);
#784=FACE_BOUND('',#2072,.T.);
#785=FACE_BOUND('',#2073,.T.);
#786=FACE_BOUND('',#2077,.T.);
#787=FACE_BOUND('',#2079,.T.);
#788=FACE_BOUND('',#2085,.T.);
#789=FACE_BOUND('',#2092,.T.);
#790=FACE_BOUND('',#2095,.T.);
#791=FACE_BOUND('',#2101,.T.);
#792=FACE_BOUND('',#2108,.T.);
#793=FACE_BOUND('',#2111,.T.);
#794=FACE_BOUND('',#2115,.T.);
#795=FACE_BOUND('',#2123,.T.);
#796=FACE_BOUND('',#2127,.T.);
#797=FACE_BOUND('',#2131,.T.);
#798=FACE_BOUND('',#2143,.T.);
#799=FACE_BOUND('',#2145,.T.);
#800=FACE_BOUND('',#2151,.T.);
#801=FACE_BOUND('',#2155,.T.);
#802=FACE_BOUND('',#2167,.T.);
#803=FACE_BOUND('',#2169,.T.);
#804=FACE_BOUND('',#2177,.T.);
#805=FACE_BOUND('',#2180,.T.);
#806=FACE_BOUND('',#2185,.T.);
#807=FACE_BOUND('',#2190,.T.);
#808=FACE_BOUND('',#2218,.T.);
#809=FACE_BOUND('',#2221,.T.);
#810=FACE_BOUND('',#2224,.T.);
#811=FACE_BOUND('',#2227,.T.);
#812=FACE_BOUND('',#2230,.T.);
#813=FACE_BOUND('',#2278,.T.);
#814=FACE_BOUND('',#2280,.T.);
#815=FACE_BOUND('',#2284,.T.);
#816=FACE_BOUND('',#2310,.T.);
#817=FACE_BOUND('',#2315,.T.);
#818=FACE_BOUND('',#2318,.T.);
#819=FACE_BOUND('',#2321,.T.);
#820=FACE_BOUND('',#2324,.T.);
#821=FACE_BOUND('',#2334,.T.);
#822=FACE_BOUND('',#2335,.T.);
#823=FACE_BOUND('',#2336,.T.);
#824=FACE_BOUND('',#2337,.T.);
#825=FACE_BOUND('',#2344,.T.);
#826=FACE_BOUND('',#2345,.T.);
#827=FACE_BOUND('',#2346,.T.);
#828=FACE_BOUND('',#2347,.T.);
#829=FACE_BOUND('',#2354,.T.);
#830=FACE_BOUND('',#2356,.T.);
#831=FACE_BOUND('',#2361,.T.);
#832=FACE_BOUND('',#2365,.T.);
#833=FACE_BOUND('',#2368,.T.);
#834=FACE_BOUND('',#2372,.T.);
#835=FACE_BOUND('',#2374,.T.);
#836=FACE_BOUND('',#2378,.T.);
#837=FACE_BOUND('',#2380,.T.);
#838=FACE_BOUND('',#2390,.T.);
#839=FACE_BOUND('',#2392,.T.);
#840=FACE_BOUND('',#2396,.T.);
#841=FACE_BOUND('',#2398,.T.);
#842=FACE_BOUND('',#2403,.T.);
#843=FACE_BOUND('',#2407,.T.);
#844=FACE_BOUND('',#2410,.T.);
#845=FACE_BOUND('',#2414,.T.);
#846=FACE_BOUND('',#2416,.T.);
#847=FACE_BOUND('',#2420,.T.);
#848=FACE_BOUND('',#2422,.T.);
#849=FACE_BOUND('',#2432,.T.);
#850=FACE_BOUND('',#2434,.T.);
#851=FACE_BOUND('',#2438,.T.);
#852=FACE_BOUND('',#2439,.T.);
#853=FACE_BOUND('',#2440,.T.);
#854=FACE_BOUND('',#2444,.T.);
#855=FACE_BOUND('',#2445,.T.);
#856=FACE_BOUND('',#2446,.T.);
#857=FACE_BOUND('',#2448,.T.);
#858=FACE_BOUND('',#2450,.T.);
#859=FACE_BOUND('',#2453,.T.);
#860=FACE_BOUND('',#2455,.T.);
#861=FACE_BOUND('',#2458,.T.);
#862=FACE_BOUND('',#2501,.T.);
#863=FACE_BOUND('',#2504,.T.);
#864=FACE_BOUND('',#2516,.T.);
#865=FACE_BOUND('',#2517,.T.);
#866=FACE_BOUND('',#2518,.T.);
#867=FACE_BOUND('',#2519,.T.);
#868=FACE_BOUND('',#2520,.T.);
#869=FACE_BOUND('',#2521,.T.);
#870=FACE_BOUND('',#2523,.T.);
#871=FACE_BOUND('',#2524,.T.);
#872=FACE_BOUND('',#2525,.T.);
#873=FACE_BOUND('',#2526,.T.);
#874=FACE_BOUND('',#2527,.T.);
#875=FACE_BOUND('',#2528,.T.);
#876=FACE_BOUND('',#2544,.T.);
#877=FACE_BOUND('',#2545,.T.);
#878=FACE_BOUND('',#2551,.T.);
#879=FACE_BOUND('',#2552,.T.);
#880=FACE_BOUND('',#2573,.T.);
#881=FACE_BOUND('',#2574,.T.);
#882=FACE_BOUND('',#2575,.T.);
#883=FACE_BOUND('',#2576,.T.);
#884=FACE_BOUND('',#2608,.T.);
#885=FACE_BOUND('',#2611,.T.);
#886=FACE_BOUND('',#2617,.T.);
#887=FACE_BOUND('',#2644,.T.);
#888=FACE_BOUND('',#2652,.T.);
#889=PLANE('',#11496);
#890=PLANE('',#11500);
#891=PLANE('',#11504);
#892=PLANE('',#11508);
#893=PLANE('',#11512);
#894=PLANE('',#11516);
#895=PLANE('',#11520);
#896=PLANE('',#11524);
#897=PLANE('',#11540);
#898=PLANE('',#11544);
#899=PLANE('',#11548);
#900=PLANE('',#11552);
#901=PLANE('',#11556);
#902=PLANE('',#11560);
#903=PLANE('',#11564);
#904=PLANE('',#11568);
#905=PLANE('',#11569);
#906=PLANE('',#11570);
#907=PLANE('',#11571);
#908=PLANE('',#11572);
#909=PLANE('',#11573);
#910=PLANE('',#11574);
#911=PLANE('',#11576);
#912=PLANE('',#11577);
#913=PLANE('',#11578);
#914=PLANE('',#11579);
#915=PLANE('',#11580);
#916=PLANE('',#11581);
#917=PLANE('',#11582);
#918=PLANE('',#11583);
#919=PLANE('',#11584);
#920=PLANE('',#11585);
#921=PLANE('',#11586);
#922=PLANE('',#11587);
#923=PLANE('',#11589);
#924=PLANE('',#11590);
#925=PLANE('',#11591);
#926=PLANE('',#11592);
#927=PLANE('',#11593);
#928=PLANE('',#11594);
#929=PLANE('',#11595);
#930=PLANE('',#11596);
#931=PLANE('',#11597);
#932=PLANE('',#11598);
#933=PLANE('',#11599);
#934=PLANE('',#11600);
#935=PLANE('',#11629);
#936=PLANE('',#11630);
#937=PLANE('',#11631);
#938=PLANE('',#11632);
#939=PLANE('',#11633);
#940=PLANE('',#11634);
#941=PLANE('',#11635);
#942=PLANE('',#11636);
#943=PLANE('',#11637);
#944=PLANE('',#11638);
#945=PLANE('',#11646);
#946=PLANE('',#11647);
#947=PLANE('',#11661);
#948=PLANE('',#11678);
#949=PLANE('',#11681);
#950=PLANE('',#11695);
#951=PLANE('',#11711);
#952=PLANE('',#11715);
#953=PLANE('',#11744);
#954=PLANE('',#11745);
#955=PLANE('',#11746);
#956=PLANE('',#11747);
#957=PLANE('',#11748);
#958=PLANE('',#11749);
#959=PLANE('',#11750);
#960=PLANE('',#11751);
#961=PLANE('',#11752);
#962=PLANE('',#11753);
#963=PLANE('',#11761);
#964=PLANE('',#11762);
#965=PLANE('',#11776);
#966=PLANE('',#11793);
#967=PLANE('',#11796);
#968=PLANE('',#11810);
#969=PLANE('',#11826);
#970=PLANE('',#11830);
#971=PLANE('',#11832);
#972=PLANE('',#11833);
#973=PLANE('',#11834);
#974=PLANE('',#11845);
#975=PLANE('',#11846);
#976=PLANE('',#11849);
#977=PLANE('',#11857);
#978=PLANE('',#11865);
#979=PLANE('',#11867);
#980=PLANE('',#11868);
#981=PLANE('',#11869);
#982=PLANE('',#11870);
#983=PLANE('',#11875);
#984=PLANE('',#11876);
#985=PLANE('',#11877);
#986=PLANE('',#11878);
#987=PLANE('',#11879);
#988=PLANE('',#11880);
#989=PLANE('',#11881);
#990=PLANE('',#11882);
#991=PLANE('',#11890);
#992=PLANE('',#11898);
#993=PLANE('',#11900);
#994=PLANE('',#11901);
#995=PLANE('',#11902);
#996=PLANE('',#11903);
#997=PLANE('',#11908);
#998=PLANE('',#11909);
#999=PLANE('',#11910);
#1000=PLANE('',#11911);
#1001=PLANE('',#11912);
#1002=PLANE('',#11913);
#1003=PLANE('',#11914);
#1004=PLANE('',#11915);
#1005=PLANE('',#11931);
#1006=PLANE('',#11934);
#1007=PLANE('',#11946);
#1008=PLANE('',#11955);
#1009=PLANE('',#11988);
#1010=PLANE('',#11993);
#1011=PLANE('',#11998);
#1012=PLANE('',#12003);
#1013=PLANE('',#12008);
#1014=PLANE('',#12013);
#1015=PLANE('',#12022);
#1016=PLANE('',#12026);
#1017=PLANE('',#12027);
#1018=PLANE('',#12029);
#1019=PLANE('',#12034);
#1020=PLANE('',#12037);
#1021=PLANE('',#12042);
#1022=PLANE('',#12051);
#1023=PLANE('',#12052);
#1024=PLANE('',#12053);
#1025=PLANE('',#12054);
#1026=PLANE('',#12055);
#1027=PLANE('',#12056);
#1028=PLANE('',#12057);
#1029=PLANE('',#12058);
#1030=PLANE('',#12059);
#1031=PLANE('',#12060);
#1032=PLANE('',#12061);
#1033=PLANE('',#12062);
#1034=PLANE('',#12063);
#1035=PLANE('',#12064);
#1036=PLANE('',#12065);
#1037=PLANE('',#12066);
#1038=PLANE('',#12067);
#1039=PLANE('',#12068);
#1040=PLANE('',#12069);
#1041=PLANE('',#12070);
#1042=PLANE('',#12071);
#1043=PLANE('',#12072);
#1044=PLANE('',#12073);
#1045=PLANE('',#12074);
#1046=PLANE('',#12075);
#1047=PLANE('',#12076);
#1048=PLANE('',#12077);
#1049=PLANE('',#12078);
#1050=PLANE('',#12079);
#1051=PLANE('',#12080);
#1052=PLANE('',#12081);
#1053=PLANE('',#12082);
#1054=PLANE('',#12083);
#1055=PLANE('',#12084);
#1056=PLANE('',#12085);
#1057=PLANE('',#12086);
#1058=PLANE('',#12090);
#1059=PLANE('',#12091);
#1060=PLANE('',#12092);
#1061=PLANE('',#12093);
#1062=PLANE('',#12094);
#1063=PLANE('',#12095);
#1064=PLANE('',#12096);
#1065=PLANE('',#12097);
#1066=PLANE('',#12098);
#1067=PLANE('',#12099);
#1068=PLANE('',#12101);
#1069=PLANE('',#12102);
#1070=PLANE('',#12103);
#1071=PLANE('',#12105);
#1072=PLANE('',#12106);
#1073=PLANE('',#12107);
#1074=PLANE('',#12108);
#1075=PLANE('',#12109);
#1076=PLANE('',#12110);
#1077=PLANE('',#12117);
#1078=PLANE('',#12118);
#1079=PLANE('',#12119);
#1080=PLANE('',#12120);
#1081=PLANE('',#12122);
#1082=PLANE('',#12123);
#1083=PLANE('',#12124);
#1084=PLANE('',#12125);
#1085=PLANE('',#12126);
#1086=PLANE('',#12127);
#1087=PLANE('',#12128);
#1088=PLANE('',#12129);
#1089=PLANE('',#12130);
#1090=PLANE('',#12132);
#1091=PLANE('',#12140);
#1092=PLANE('',#12149);
#1093=PLANE('',#12154);
#1094=PLANE('',#12159);
#1095=PLANE('',#12164);
#1096=PLANE('',#12174);
#1097=PLANE('',#12175);
#1098=PLANE('',#12176);
#1099=PLANE('',#12177);
#1100=PLANE('',#12178);
#1101=PLANE('',#12179);
#1102=PLANE('',#12180);
#1103=PLANE('',#12181);
#1104=PLANE('',#12182);
#1105=PLANE('',#12183);
#1106=PLANE('',#12184);
#1107=PLANE('',#12185);
#1108=PLANE('',#12186);
#1109=PLANE('',#12187);
#1110=PLANE('',#12193);
#1111=PLANE('',#12194);
#1112=PLANE('',#12197);
#1113=PLANE('',#12206);
#1114=PLANE('',#12209);
#1115=PLANE('',#12210);
#1116=PLANE('',#12215);
#1117=PLANE('',#12222);
#1118=PLANE('',#12223);
#1119=PLANE('',#12231);
#1120=PLANE('',#12232);
#1121=PLANE('',#12237);
#1122=PLANE('',#12238);
#1123=PLANE('',#12243);
#1124=PLANE('',#12244);
#1125=PLANE('',#12252);
#1126=PLANE('',#12253);
#1127=PLANE('',#12259);
#1128=PLANE('',#12260);
#1129=PLANE('',#12263);
#1130=PLANE('',#12272);
#1131=PLANE('',#12275);
#1132=PLANE('',#12276);
#1133=PLANE('',#12281);
#1134=PLANE('',#12288);
#1135=PLANE('',#12289);
#1136=PLANE('',#12297);
#1137=PLANE('',#12298);
#1138=PLANE('',#12303);
#1139=PLANE('',#12304);
#1140=PLANE('',#12309);
#1141=PLANE('',#12310);
#1142=PLANE('',#12318);
#1143=PLANE('',#12319);
#1144=PLANE('',#12331);
#1145=PLANE('',#12332);
#1146=PLANE('',#12376);
#1147=PLANE('',#12377);
#1148=PLANE('',#12421);
#1149=PLANE('',#12467);
#1150=PLANE('',#12472);
#1151=PLANE('',#12490);
#1152=PLANE('',#12491);
#1153=PLANE('',#12492);
#1154=PLANE('',#12493);
#1155=PLANE('',#12494);
#1156=PLANE('',#12495);
#1157=PLANE('',#12500);
#1158=PLANE('',#12504);
#1159=PLANE('',#12505);
#1160=PLANE('',#12512);
#1161=PLANE('',#12513);
#1162=PLANE('',#12514);
#1163=PLANE('',#12518);
#1164=PLANE('',#12522);
#1165=PLANE('',#12523);
#1166=PLANE('',#12524);
#1167=PLANE('',#12525);
#1168=PLANE('',#12526);
#1169=PLANE('',#12527);
#1170=PLANE('',#12528);
#1171=PLANE('',#12530);
#1172=PLANE('',#12531);
#1173=PLANE('',#12532);
#1174=PLANE('',#12533);
#1175=PLANE('',#12534);
#1176=PLANE('',#12535);
#1177=PLANE('',#12538);
#1178=PLANE('',#12544);
#1179=PLANE('',#12550);
#1180=PLANE('',#12556);
#1181=PLANE('',#12562);
#1182=PLANE('',#12563);
#1183=PLANE('',#12564);
#1184=PLANE('',#12565);
#1185=PLANE('',#12566);
#1186=PLANE('',#12567);
#1187=PLANE('',#12568);
#1188=PLANE('',#12569);
#1189=PLANE('',#12570);
#1190=PLANE('',#12571);
#1191=PLANE('',#12572);
#1192=PLANE('',#12573);
#1193=PLANE('',#12574);
#1194=PLANE('',#12575);
#1195=PLANE('',#12577);
#1196=PLANE('',#12578);
#1197=PLANE('',#12579);
#1198=PLANE('',#12580);
#1199=PLANE('',#12581);
#1200=PLANE('',#12582);
#1201=PLANE('',#12583);
#1202=PLANE('',#12584);
#1203=PLANE('',#12585);
#1204=PLANE('',#12586);
#1205=PLANE('',#12588);
#1206=PLANE('',#12589);
#1207=PLANE('',#12590);
#1208=PLANE('',#12591);
#1209=PLANE('',#12592);
#1210=PLANE('',#12593);
#1211=PLANE('',#12594);
#1212=PLANE('',#12595);
#1213=PLANE('',#12596);
#1214=PLANE('',#12597);
#1215=PLANE('',#12607);
#1216=PLANE('',#12611);
#1217=PLANE('',#12613);
#1218=PLANE('',#12621);
#1219=PLANE('',#12629);
#1220=PLANE('',#12630);
#1221=PLANE('',#12631);
#1222=PLANE('',#12632);
#1223=PLANE('',#12633);
#1224=PLANE('',#12634);
#1225=PLANE('',#12635);
#1226=PLANE('',#12636);
#1227=PLANE('',#12637);
#1228=PLANE('',#12639);
#1229=PLANE('',#12640);
#1230=PLANE('',#12641);
#1231=PLANE('',#12642);
#1232=PLANE('',#12643);
#1233=PLANE('',#12644);
#1234=PLANE('',#12645);
#1235=PLANE('',#12646);
#1236=PLANE('',#12647);
#1237=PLANE('',#12649);
#1238=PLANE('',#12657);
#1239=PLANE('',#12663);
#1240=PLANE('',#12671);
#1241=PLANE('',#12679);
#1242=PLANE('',#12680);
#1243=PLANE('',#12681);
#1244=PLANE('',#12682);
#1245=PLANE('',#12683);
#1246=PLANE('',#12684);
#1247=PLANE('',#12685);
#1248=PLANE('',#12686);
#1249=PLANE('',#12687);
#1250=FACE_OUTER_BOUND('',#1872,.T.);
#1251=FACE_OUTER_BOUND('',#1873,.T.);
#1252=FACE_OUTER_BOUND('',#1874,.T.);
#1253=FACE_OUTER_BOUND('',#1875,.T.);
#1254=FACE_OUTER_BOUND('',#1876,.T.);
#1255=FACE_OUTER_BOUND('',#1877,.T.);
#1256=FACE_OUTER_BOUND('',#1878,.T.);
#1257=FACE_OUTER_BOUND('',#1879,.T.);
#1258=FACE_OUTER_BOUND('',#1880,.T.);
#1259=FACE_OUTER_BOUND('',#1881,.T.);
#1260=FACE_OUTER_BOUND('',#1882,.T.);
#1261=FACE_OUTER_BOUND('',#1883,.T.);
#1262=FACE_OUTER_BOUND('',#1884,.T.);
#1263=FACE_OUTER_BOUND('',#1885,.T.);
#1264=FACE_OUTER_BOUND('',#1886,.T.);
#1265=FACE_OUTER_BOUND('',#1887,.T.);
#1266=FACE_OUTER_BOUND('',#1888,.T.);
#1267=FACE_OUTER_BOUND('',#1889,.T.);
#1268=FACE_OUTER_BOUND('',#1890,.T.);
#1269=FACE_OUTER_BOUND('',#1891,.T.);
#1270=FACE_OUTER_BOUND('',#1892,.T.);
#1271=FACE_OUTER_BOUND('',#1893,.T.);
#1272=FACE_OUTER_BOUND('',#1894,.T.);
#1273=FACE_OUTER_BOUND('',#1895,.T.);
#1274=FACE_OUTER_BOUND('',#1896,.T.);
#1275=FACE_OUTER_BOUND('',#1897,.T.);
#1276=FACE_OUTER_BOUND('',#1898,.T.);
#1277=FACE_OUTER_BOUND('',#1899,.T.);
#1278=FACE_OUTER_BOUND('',#1900,.T.);
#1279=FACE_OUTER_BOUND('',#1901,.T.);
#1280=FACE_OUTER_BOUND('',#1902,.T.);
#1281=FACE_OUTER_BOUND('',#1903,.T.);
#1282=FACE_OUTER_BOUND('',#1904,.T.);
#1283=FACE_OUTER_BOUND('',#1905,.T.);
#1284=FACE_OUTER_BOUND('',#1906,.T.);
#1285=FACE_OUTER_BOUND('',#1907,.T.);
#1286=FACE_OUTER_BOUND('',#1908,.T.);
#1287=FACE_OUTER_BOUND('',#1909,.T.);
#1288=FACE_OUTER_BOUND('',#1910,.T.);
#1289=FACE_OUTER_BOUND('',#1911,.T.);
#1290=FACE_OUTER_BOUND('',#1912,.T.);
#1291=FACE_OUTER_BOUND('',#1933,.T.);
#1292=FACE_OUTER_BOUND('',#1938,.T.);
#1293=FACE_OUTER_BOUND('',#1939,.T.);
#1294=FACE_OUTER_BOUND('',#1940,.T.);
#1295=FACE_OUTER_BOUND('',#1941,.T.);
#1296=FACE_OUTER_BOUND('',#1942,.T.);
#1297=FACE_OUTER_BOUND('',#1943,.T.);
#1298=FACE_OUTER_BOUND('',#1944,.T.);
#1299=FACE_OUTER_BOUND('',#1945,.T.);
#1300=FACE_OUTER_BOUND('',#1946,.T.);
#1301=FACE_OUTER_BOUND('',#1947,.T.);
#1302=FACE_OUTER_BOUND('',#1948,.T.);
#1303=FACE_OUTER_BOUND('',#1949,.T.);
#1304=FACE_OUTER_BOUND('',#1950,.T.);
#1305=FACE_OUTER_BOUND('',#1951,.T.);
#1306=FACE_OUTER_BOUND('',#1952,.T.);
#1307=FACE_OUTER_BOUND('',#1953,.T.);
#1308=FACE_OUTER_BOUND('',#1954,.T.);
#1309=FACE_OUTER_BOUND('',#1955,.T.);
#1310=FACE_OUTER_BOUND('',#1956,.T.);
#1311=FACE_OUTER_BOUND('',#1957,.T.);
#1312=FACE_OUTER_BOUND('',#1958,.T.);
#1313=FACE_OUTER_BOUND('',#1959,.T.);
#1314=FACE_OUTER_BOUND('',#1960,.T.);
#1315=FACE_OUTER_BOUND('',#1961,.T.);
#1316=FACE_OUTER_BOUND('',#1962,.T.);
#1317=FACE_OUTER_BOUND('',#1963,.T.);
#1318=FACE_OUTER_BOUND('',#1964,.T.);
#1319=FACE_OUTER_BOUND('',#1965,.T.);
#1320=FACE_OUTER_BOUND('',#1966,.T.);
#1321=FACE_OUTER_BOUND('',#1967,.T.);
#1322=FACE_OUTER_BOUND('',#1968,.T.);
#1323=FACE_OUTER_BOUND('',#1969,.T.);
#1324=FACE_OUTER_BOUND('',#1970,.T.);
#1325=FACE_OUTER_BOUND('',#1971,.T.);
#1326=FACE_OUTER_BOUND('',#1974,.T.);
#1327=FACE_OUTER_BOUND('',#1977,.T.);
#1328=FACE_OUTER_BOUND('',#1978,.T.);
#1329=FACE_OUTER_BOUND('',#1979,.T.);
#1330=FACE_OUTER_BOUND('',#1985,.T.);
#1331=FACE_OUTER_BOUND('',#1986,.T.);
#1332=FACE_OUTER_BOUND('',#1992,.T.);
#1333=FACE_OUTER_BOUND('',#1993,.T.);
#1334=FACE_OUTER_BOUND('',#1994,.T.);
#1335=FACE_OUTER_BOUND('',#1999,.T.);
#1336=FACE_OUTER_BOUND('',#2000,.T.);
#1337=FACE_OUTER_BOUND('',#2001,.T.);
#1338=FACE_OUTER_BOUND('',#2003,.T.);
#1339=FACE_OUTER_BOUND('',#2005,.T.);
#1340=FACE_OUTER_BOUND('',#2006,.T.);
#1341=FACE_OUTER_BOUND('',#2007,.T.);
#1342=FACE_OUTER_BOUND('',#2008,.T.);
#1343=FACE_OUTER_BOUND('',#2009,.T.);
#1344=FACE_OUTER_BOUND('',#2011,.T.);
#1345=FACE_OUTER_BOUND('',#2012,.T.);
#1346=FACE_OUTER_BOUND('',#2013,.T.);
#1347=FACE_OUTER_BOUND('',#2014,.T.);
#1348=FACE_OUTER_BOUND('',#2015,.T.);
#1349=FACE_OUTER_BOUND('',#2016,.T.);
#1350=FACE_OUTER_BOUND('',#2018,.T.);
#1351=FACE_OUTER_BOUND('',#2019,.T.);
#1352=FACE_OUTER_BOUND('',#2021,.T.);
#1353=FACE_OUTER_BOUND('',#2022,.T.);
#1354=FACE_OUTER_BOUND('',#2023,.T.);
#1355=FACE_OUTER_BOUND('',#2024,.T.);
#1356=FACE_OUTER_BOUND('',#2025,.T.);
#1357=FACE_OUTER_BOUND('',#2027,.T.);
#1358=FACE_OUTER_BOUND('',#2028,.T.);
#1359=FACE_OUTER_BOUND('',#2029,.T.);
#1360=FACE_OUTER_BOUND('',#2030,.T.);
#1361=FACE_OUTER_BOUND('',#2031,.T.);
#1362=FACE_OUTER_BOUND('',#2032,.T.);
#1363=FACE_OUTER_BOUND('',#2034,.T.);
#1364=FACE_OUTER_BOUND('',#2035,.T.);
#1365=FACE_OUTER_BOUND('',#2037,.T.);
#1366=FACE_OUTER_BOUND('',#2038,.T.);
#1367=FACE_OUTER_BOUND('',#2039,.T.);
#1368=FACE_OUTER_BOUND('',#2040,.T.);
#1369=FACE_OUTER_BOUND('',#2041,.T.);
#1370=FACE_OUTER_BOUND('',#2042,.T.);
#1371=FACE_OUTER_BOUND('',#2043,.T.);
#1372=FACE_OUTER_BOUND('',#2044,.T.);
#1373=FACE_OUTER_BOUND('',#2045,.T.);
#1374=FACE_OUTER_BOUND('',#2046,.T.);
#1375=FACE_OUTER_BOUND('',#2049,.T.);
#1376=FACE_OUTER_BOUND('',#2052,.T.);
#1377=FACE_OUTER_BOUND('',#2053,.T.);
#1378=FACE_OUTER_BOUND('',#2054,.T.);
#1379=FACE_OUTER_BOUND('',#2060,.T.);
#1380=FACE_OUTER_BOUND('',#2061,.T.);
#1381=FACE_OUTER_BOUND('',#2067,.T.);
#1382=FACE_OUTER_BOUND('',#2068,.T.);
#1383=FACE_OUTER_BOUND('',#2069,.T.);
#1384=FACE_OUTER_BOUND('',#2074,.T.);
#1385=FACE_OUTER_BOUND('',#2075,.T.);
#1386=FACE_OUTER_BOUND('',#2076,.T.);
#1387=FACE_OUTER_BOUND('',#2078,.T.);
#1388=FACE_OUTER_BOUND('',#2080,.T.);
#1389=FACE_OUTER_BOUND('',#2081,.T.);
#1390=FACE_OUTER_BOUND('',#2082,.T.);
#1391=FACE_OUTER_BOUND('',#2083,.T.);
#1392=FACE_OUTER_BOUND('',#2084,.T.);
#1393=FACE_OUTER_BOUND('',#2086,.T.);
#1394=FACE_OUTER_BOUND('',#2087,.T.);
#1395=FACE_OUTER_BOUND('',#2088,.T.);
#1396=FACE_OUTER_BOUND('',#2089,.T.);
#1397=FACE_OUTER_BOUND('',#2090,.T.);
#1398=FACE_OUTER_BOUND('',#2091,.T.);
#1399=FACE_OUTER_BOUND('',#2093,.T.);
#1400=FACE_OUTER_BOUND('',#2094,.T.);
#1401=FACE_OUTER_BOUND('',#2096,.T.);
#1402=FACE_OUTER_BOUND('',#2097,.T.);
#1403=FACE_OUTER_BOUND('',#2098,.T.);
#1404=FACE_OUTER_BOUND('',#2099,.T.);
#1405=FACE_OUTER_BOUND('',#2100,.T.);
#1406=FACE_OUTER_BOUND('',#2102,.T.);
#1407=FACE_OUTER_BOUND('',#2103,.T.);
#1408=FACE_OUTER_BOUND('',#2104,.T.);
#1409=FACE_OUTER_BOUND('',#2105,.T.);
#1410=FACE_OUTER_BOUND('',#2106,.T.);
#1411=FACE_OUTER_BOUND('',#2107,.T.);
#1412=FACE_OUTER_BOUND('',#2109,.T.);
#1413=FACE_OUTER_BOUND('',#2110,.T.);
#1414=FACE_OUTER_BOUND('',#2112,.T.);
#1415=FACE_OUTER_BOUND('',#2113,.T.);
#1416=FACE_OUTER_BOUND('',#2114,.T.);
#1417=FACE_OUTER_BOUND('',#2116,.T.);
#1418=FACE_OUTER_BOUND('',#2117,.T.);
#1419=FACE_OUTER_BOUND('',#2118,.T.);
#1420=FACE_OUTER_BOUND('',#2119,.T.);
#1421=FACE_OUTER_BOUND('',#2120,.T.);
#1422=FACE_OUTER_BOUND('',#2121,.T.);
#1423=FACE_OUTER_BOUND('',#2122,.T.);
#1424=FACE_OUTER_BOUND('',#2124,.T.);
#1425=FACE_OUTER_BOUND('',#2125,.T.);
#1426=FACE_OUTER_BOUND('',#2126,.T.);
#1427=FACE_OUTER_BOUND('',#2128,.T.);
#1428=FACE_OUTER_BOUND('',#2129,.T.);
#1429=FACE_OUTER_BOUND('',#2130,.T.);
#1430=FACE_OUTER_BOUND('',#2132,.T.);
#1431=FACE_OUTER_BOUND('',#2133,.T.);
#1432=FACE_OUTER_BOUND('',#2134,.T.);
#1433=FACE_OUTER_BOUND('',#2135,.T.);
#1434=FACE_OUTER_BOUND('',#2136,.T.);
#1435=FACE_OUTER_BOUND('',#2137,.T.);
#1436=FACE_OUTER_BOUND('',#2138,.T.);
#1437=FACE_OUTER_BOUND('',#2139,.T.);
#1438=FACE_OUTER_BOUND('',#2140,.T.);
#1439=FACE_OUTER_BOUND('',#2141,.T.);
#1440=FACE_OUTER_BOUND('',#2142,.T.);
#1441=FACE_OUTER_BOUND('',#2144,.T.);
#1442=FACE_OUTER_BOUND('',#2146,.T.);
#1443=FACE_OUTER_BOUND('',#2147,.T.);
#1444=FACE_OUTER_BOUND('',#2148,.T.);
#1445=FACE_OUTER_BOUND('',#2149,.T.);
#1446=FACE_OUTER_BOUND('',#2150,.T.);
#1447=FACE_OUTER_BOUND('',#2152,.T.);
#1448=FACE_OUTER_BOUND('',#2153,.T.);
#1449=FACE_OUTER_BOUND('',#2154,.T.);
#1450=FACE_OUTER_BOUND('',#2156,.T.);
#1451=FACE_OUTER_BOUND('',#2157,.T.);
#1452=FACE_OUTER_BOUND('',#2158,.T.);
#1453=FACE_OUTER_BOUND('',#2159,.T.);
#1454=FACE_OUTER_BOUND('',#2160,.T.);
#1455=FACE_OUTER_BOUND('',#2161,.T.);
#1456=FACE_OUTER_BOUND('',#2162,.T.);
#1457=FACE_OUTER_BOUND('',#2163,.T.);
#1458=FACE_OUTER_BOUND('',#2164,.T.);
#1459=FACE_OUTER_BOUND('',#2165,.T.);
#1460=FACE_OUTER_BOUND('',#2166,.T.);
#1461=FACE_OUTER_BOUND('',#2168,.T.);
#1462=FACE_OUTER_BOUND('',#2170,.T.);
#1463=FACE_OUTER_BOUND('',#2171,.T.);
#1464=FACE_OUTER_BOUND('',#2172,.T.);
#1465=FACE_OUTER_BOUND('',#2173,.T.);
#1466=FACE_OUTER_BOUND('',#2174,.T.);
#1467=FACE_OUTER_BOUND('',#2175,.T.);
#1468=FACE_OUTER_BOUND('',#2176,.T.);
#1469=FACE_OUTER_BOUND('',#2178,.T.);
#1470=FACE_OUTER_BOUND('',#2179,.T.);
#1471=FACE_OUTER_BOUND('',#2181,.T.);
#1472=FACE_OUTER_BOUND('',#2182,.T.);
#1473=FACE_OUTER_BOUND('',#2183,.T.);
#1474=FACE_OUTER_BOUND('',#2184,.T.);
#1475=FACE_OUTER_BOUND('',#2186,.T.);
#1476=FACE_OUTER_BOUND('',#2187,.T.);
#1477=FACE_OUTER_BOUND('',#2188,.T.);
#1478=FACE_OUTER_BOUND('',#2189,.T.);
#1479=FACE_OUTER_BOUND('',#2191,.T.);
#1480=FACE_OUTER_BOUND('',#2192,.T.);
#1481=FACE_OUTER_BOUND('',#2193,.T.);
#1482=FACE_OUTER_BOUND('',#2194,.T.);
#1483=FACE_OUTER_BOUND('',#2195,.T.);
#1484=FACE_OUTER_BOUND('',#2196,.T.);
#1485=FACE_OUTER_BOUND('',#2197,.T.);
#1486=FACE_OUTER_BOUND('',#2198,.T.);
#1487=FACE_OUTER_BOUND('',#2199,.T.);
#1488=FACE_OUTER_BOUND('',#2200,.T.);
#1489=FACE_OUTER_BOUND('',#2201,.T.);
#1490=FACE_OUTER_BOUND('',#2202,.T.);
#1491=FACE_OUTER_BOUND('',#2203,.T.);
#1492=FACE_OUTER_BOUND('',#2204,.T.);
#1493=FACE_OUTER_BOUND('',#2205,.T.);
#1494=FACE_OUTER_BOUND('',#2206,.T.);
#1495=FACE_OUTER_BOUND('',#2207,.T.);
#1496=FACE_OUTER_BOUND('',#2208,.T.);
#1497=FACE_OUTER_BOUND('',#2209,.T.);
#1498=FACE_OUTER_BOUND('',#2210,.T.);
#1499=FACE_OUTER_BOUND('',#2211,.T.);
#1500=FACE_OUTER_BOUND('',#2212,.T.);
#1501=FACE_OUTER_BOUND('',#2213,.T.);
#1502=FACE_OUTER_BOUND('',#2214,.T.);
#1503=FACE_OUTER_BOUND('',#2215,.T.);
#1504=FACE_OUTER_BOUND('',#2216,.T.);
#1505=FACE_OUTER_BOUND('',#2217,.T.);
#1506=FACE_OUTER_BOUND('',#2219,.T.);
#1507=FACE_OUTER_BOUND('',#2220,.T.);
#1508=FACE_OUTER_BOUND('',#2222,.T.);
#1509=FACE_OUTER_BOUND('',#2223,.T.);
#1510=FACE_OUTER_BOUND('',#2225,.T.);
#1511=FACE_OUTER_BOUND('',#2226,.T.);
#1512=FACE_OUTER_BOUND('',#2228,.T.);
#1513=FACE_OUTER_BOUND('',#2229,.T.);
#1514=FACE_OUTER_BOUND('',#2231,.T.);
#1515=FACE_OUTER_BOUND('',#2232,.T.);
#1516=FACE_OUTER_BOUND('',#2233,.T.);
#1517=FACE_OUTER_BOUND('',#2234,.T.);
#1518=FACE_OUTER_BOUND('',#2235,.T.);
#1519=FACE_OUTER_BOUND('',#2236,.T.);
#1520=FACE_OUTER_BOUND('',#2237,.T.);
#1521=FACE_OUTER_BOUND('',#2238,.T.);
#1522=FACE_OUTER_BOUND('',#2239,.T.);
#1523=FACE_OUTER_BOUND('',#2240,.T.);
#1524=FACE_OUTER_BOUND('',#2241,.T.);
#1525=FACE_OUTER_BOUND('',#2242,.T.);
#1526=FACE_OUTER_BOUND('',#2243,.T.);
#1527=FACE_OUTER_BOUND('',#2244,.T.);
#1528=FACE_OUTER_BOUND('',#2245,.T.);
#1529=FACE_OUTER_BOUND('',#2246,.T.);
#1530=FACE_OUTER_BOUND('',#2247,.T.);
#1531=FACE_OUTER_BOUND('',#2248,.T.);
#1532=FACE_OUTER_BOUND('',#2249,.T.);
#1533=FACE_OUTER_BOUND('',#2250,.T.);
#1534=FACE_OUTER_BOUND('',#2251,.T.);
#1535=FACE_OUTER_BOUND('',#2252,.T.);
#1536=FACE_OUTER_BOUND('',#2253,.T.);
#1537=FACE_OUTER_BOUND('',#2254,.T.);
#1538=FACE_OUTER_BOUND('',#2255,.T.);
#1539=FACE_OUTER_BOUND('',#2256,.T.);
#1540=FACE_OUTER_BOUND('',#2257,.T.);
#1541=FACE_OUTER_BOUND('',#2258,.T.);
#1542=FACE_OUTER_BOUND('',#2259,.T.);
#1543=FACE_OUTER_BOUND('',#2260,.T.);
#1544=FACE_OUTER_BOUND('',#2261,.T.);
#1545=FACE_OUTER_BOUND('',#2262,.T.);
#1546=FACE_OUTER_BOUND('',#2263,.T.);
#1547=FACE_OUTER_BOUND('',#2264,.T.);
#1548=FACE_OUTER_BOUND('',#2265,.T.);
#1549=FACE_OUTER_BOUND('',#2266,.T.);
#1550=FACE_OUTER_BOUND('',#2267,.T.);
#1551=FACE_OUTER_BOUND('',#2268,.T.);
#1552=FACE_OUTER_BOUND('',#2269,.T.);
#1553=FACE_OUTER_BOUND('',#2270,.T.);
#1554=FACE_OUTER_BOUND('',#2271,.T.);
#1555=FACE_OUTER_BOUND('',#2272,.T.);
#1556=FACE_OUTER_BOUND('',#2273,.T.);
#1557=FACE_OUTER_BOUND('',#2274,.T.);
#1558=FACE_OUTER_BOUND('',#2275,.T.);
#1559=FACE_OUTER_BOUND('',#2276,.T.);
#1560=FACE_OUTER_BOUND('',#2277,.T.);
#1561=FACE_OUTER_BOUND('',#2279,.T.);
#1562=FACE_OUTER_BOUND('',#2281,.T.);
#1563=FACE_OUTER_BOUND('',#2282,.T.);
#1564=FACE_OUTER_BOUND('',#2283,.T.);
#1565=FACE_OUTER_BOUND('',#2285,.T.);
#1566=FACE_OUTER_BOUND('',#2286,.T.);
#1567=FACE_OUTER_BOUND('',#2287,.T.);
#1568=FACE_OUTER_BOUND('',#2288,.T.);
#1569=FACE_OUTER_BOUND('',#2289,.T.);
#1570=FACE_OUTER_BOUND('',#2290,.T.);
#1571=FACE_OUTER_BOUND('',#2291,.T.);
#1572=FACE_OUTER_BOUND('',#2292,.T.);
#1573=FACE_OUTER_BOUND('',#2293,.T.);
#1574=FACE_OUTER_BOUND('',#2294,.T.);
#1575=FACE_OUTER_BOUND('',#2295,.T.);
#1576=FACE_OUTER_BOUND('',#2296,.T.);
#1577=FACE_OUTER_BOUND('',#2297,.T.);
#1578=FACE_OUTER_BOUND('',#2298,.T.);
#1579=FACE_OUTER_BOUND('',#2299,.T.);
#1580=FACE_OUTER_BOUND('',#2300,.T.);
#1581=FACE_OUTER_BOUND('',#2301,.T.);
#1582=FACE_OUTER_BOUND('',#2302,.T.);
#1583=FACE_OUTER_BOUND('',#2303,.T.);
#1584=FACE_OUTER_BOUND('',#2304,.T.);
#1585=FACE_OUTER_BOUND('',#2305,.T.);
#1586=FACE_OUTER_BOUND('',#2306,.T.);
#1587=FACE_OUTER_BOUND('',#2307,.T.);
#1588=FACE_OUTER_BOUND('',#2308,.T.);
#1589=FACE_OUTER_BOUND('',#2309,.T.);
#1590=FACE_OUTER_BOUND('',#2311,.T.);
#1591=FACE_OUTER_BOUND('',#2312,.T.);
#1592=FACE_OUTER_BOUND('',#2313,.T.);
#1593=FACE_OUTER_BOUND('',#2314,.T.);
#1594=FACE_OUTER_BOUND('',#2316,.T.);
#1595=FACE_OUTER_BOUND('',#2317,.T.);
#1596=FACE_OUTER_BOUND('',#2319,.T.);
#1597=FACE_OUTER_BOUND('',#2320,.T.);
#1598=FACE_OUTER_BOUND('',#2322,.T.);
#1599=FACE_OUTER_BOUND('',#2323,.T.);
#1600=FACE_OUTER_BOUND('',#2325,.T.);
#1601=FACE_OUTER_BOUND('',#2326,.T.);
#1602=FACE_OUTER_BOUND('',#2327,.T.);
#1603=FACE_OUTER_BOUND('',#2328,.T.);
#1604=FACE_OUTER_BOUND('',#2329,.T.);
#1605=FACE_OUTER_BOUND('',#2330,.T.);
#1606=FACE_OUTER_BOUND('',#2331,.T.);
#1607=FACE_OUTER_BOUND('',#2332,.T.);
#1608=FACE_OUTER_BOUND('',#2333,.T.);
#1609=FACE_OUTER_BOUND('',#2338,.T.);
#1610=FACE_OUTER_BOUND('',#2339,.T.);
#1611=FACE_OUTER_BOUND('',#2340,.T.);
#1612=FACE_OUTER_BOUND('',#2341,.T.);
#1613=FACE_OUTER_BOUND('',#2342,.T.);
#1614=FACE_OUTER_BOUND('',#2343,.T.);
#1615=FACE_OUTER_BOUND('',#2348,.T.);
#1616=FACE_OUTER_BOUND('',#2349,.T.);
#1617=FACE_OUTER_BOUND('',#2350,.T.);
#1618=FACE_OUTER_BOUND('',#2351,.T.);
#1619=FACE_OUTER_BOUND('',#2352,.T.);
#1620=FACE_OUTER_BOUND('',#2353,.T.);
#1621=FACE_OUTER_BOUND('',#2355,.T.);
#1622=FACE_OUTER_BOUND('',#2357,.T.);
#1623=FACE_OUTER_BOUND('',#2358,.T.);
#1624=FACE_OUTER_BOUND('',#2359,.T.);
#1625=FACE_OUTER_BOUND('',#2360,.T.);
#1626=FACE_OUTER_BOUND('',#2362,.T.);
#1627=FACE_OUTER_BOUND('',#2363,.T.);
#1628=FACE_OUTER_BOUND('',#2364,.T.);
#1629=FACE_OUTER_BOUND('',#2366,.T.);
#1630=FACE_OUTER_BOUND('',#2367,.T.);
#1631=FACE_OUTER_BOUND('',#2369,.T.);
#1632=FACE_OUTER_BOUND('',#2370,.T.);
#1633=FACE_OUTER_BOUND('',#2371,.T.);
#1634=FACE_OUTER_BOUND('',#2373,.T.);
#1635=FACE_OUTER_BOUND('',#2375,.T.);
#1636=FACE_OUTER_BOUND('',#2376,.T.);
#1637=FACE_OUTER_BOUND('',#2377,.T.);
#1638=FACE_OUTER_BOUND('',#2379,.T.);
#1639=FACE_OUTER_BOUND('',#2381,.T.);
#1640=FACE_OUTER_BOUND('',#2382,.T.);
#1641=FACE_OUTER_BOUND('',#2383,.T.);
#1642=FACE_OUTER_BOUND('',#2384,.T.);
#1643=FACE_OUTER_BOUND('',#2385,.T.);
#1644=FACE_OUTER_BOUND('',#2386,.T.);
#1645=FACE_OUTER_BOUND('',#2387,.T.);
#1646=FACE_OUTER_BOUND('',#2388,.T.);
#1647=FACE_OUTER_BOUND('',#2389,.T.);
#1648=FACE_OUTER_BOUND('',#2391,.T.);
#1649=FACE_OUTER_BOUND('',#2393,.T.);
#1650=FACE_OUTER_BOUND('',#2394,.T.);
#1651=FACE_OUTER_BOUND('',#2395,.T.);
#1652=FACE_OUTER_BOUND('',#2397,.T.);
#1653=FACE_OUTER_BOUND('',#2399,.T.);
#1654=FACE_OUTER_BOUND('',#2400,.T.);
#1655=FACE_OUTER_BOUND('',#2401,.T.);
#1656=FACE_OUTER_BOUND('',#2402,.T.);
#1657=FACE_OUTER_BOUND('',#2404,.T.);
#1658=FACE_OUTER_BOUND('',#2405,.T.);
#1659=FACE_OUTER_BOUND('',#2406,.T.);
#1660=FACE_OUTER_BOUND('',#2408,.T.);
#1661=FACE_OUTER_BOUND('',#2409,.T.);
#1662=FACE_OUTER_BOUND('',#2411,.T.);
#1663=FACE_OUTER_BOUND('',#2412,.T.);
#1664=FACE_OUTER_BOUND('',#2413,.T.);
#1665=FACE_OUTER_BOUND('',#2415,.T.);
#1666=FACE_OUTER_BOUND('',#2417,.T.);
#1667=FACE_OUTER_BOUND('',#2418,.T.);
#1668=FACE_OUTER_BOUND('',#2419,.T.);
#1669=FACE_OUTER_BOUND('',#2421,.T.);
#1670=FACE_OUTER_BOUND('',#2423,.T.);
#1671=FACE_OUTER_BOUND('',#2424,.T.);
#1672=FACE_OUTER_BOUND('',#2425,.T.);
#1673=FACE_OUTER_BOUND('',#2426,.T.);
#1674=FACE_OUTER_BOUND('',#2427,.T.);
#1675=FACE_OUTER_BOUND('',#2428,.T.);
#1676=FACE_OUTER_BOUND('',#2429,.T.);
#1677=FACE_OUTER_BOUND('',#2430,.T.);
#1678=FACE_OUTER_BOUND('',#2431,.T.);
#1679=FACE_OUTER_BOUND('',#2433,.T.);
#1680=FACE_OUTER_BOUND('',#2435,.T.);
#1681=FACE_OUTER_BOUND('',#2436,.T.);
#1682=FACE_OUTER_BOUND('',#2437,.T.);
#1683=FACE_OUTER_BOUND('',#2441,.T.);
#1684=FACE_OUTER_BOUND('',#2442,.T.);
#1685=FACE_OUTER_BOUND('',#2443,.T.);
#1686=FACE_OUTER_BOUND('',#2447,.T.);
#1687=FACE_OUTER_BOUND('',#2449,.T.);
#1688=FACE_OUTER_BOUND('',#2451,.T.);
#1689=FACE_OUTER_BOUND('',#2452,.T.);
#1690=FACE_OUTER_BOUND('',#2454,.T.);
#1691=FACE_OUTER_BOUND('',#2456,.T.);
#1692=FACE_OUTER_BOUND('',#2457,.T.);
#1693=FACE_OUTER_BOUND('',#2459,.T.);
#1694=FACE_OUTER_BOUND('',#2460,.T.);
#1695=FACE_OUTER_BOUND('',#2461,.T.);
#1696=FACE_OUTER_BOUND('',#2462,.T.);
#1697=FACE_OUTER_BOUND('',#2463,.T.);
#1698=FACE_OUTER_BOUND('',#2464,.T.);
#1699=FACE_OUTER_BOUND('',#2465,.T.);
#1700=FACE_OUTER_BOUND('',#2466,.T.);
#1701=FACE_OUTER_BOUND('',#2467,.T.);
#1702=FACE_OUTER_BOUND('',#2468,.T.);
#1703=FACE_OUTER_BOUND('',#2469,.T.);
#1704=FACE_OUTER_BOUND('',#2470,.T.);
#1705=FACE_OUTER_BOUND('',#2471,.T.);
#1706=FACE_OUTER_BOUND('',#2472,.T.);
#1707=FACE_OUTER_BOUND('',#2473,.T.);
#1708=FACE_OUTER_BOUND('',#2474,.T.);
#1709=FACE_OUTER_BOUND('',#2475,.T.);
#1710=FACE_OUTER_BOUND('',#2476,.T.);
#1711=FACE_OUTER_BOUND('',#2477,.T.);
#1712=FACE_OUTER_BOUND('',#2478,.T.);
#1713=FACE_OUTER_BOUND('',#2479,.T.);
#1714=FACE_OUTER_BOUND('',#2480,.T.);
#1715=FACE_OUTER_BOUND('',#2481,.T.);
#1716=FACE_OUTER_BOUND('',#2482,.T.);
#1717=FACE_OUTER_BOUND('',#2483,.T.);
#1718=FACE_OUTER_BOUND('',#2484,.T.);
#1719=FACE_OUTER_BOUND('',#2485,.T.);
#1720=FACE_OUTER_BOUND('',#2486,.T.);
#1721=FACE_OUTER_BOUND('',#2487,.T.);
#1722=FACE_OUTER_BOUND('',#2488,.T.);
#1723=FACE_OUTER_BOUND('',#2489,.T.);
#1724=FACE_OUTER_BOUND('',#2490,.T.);
#1725=FACE_OUTER_BOUND('',#2491,.T.);
#1726=FACE_OUTER_BOUND('',#2492,.T.);
#1727=FACE_OUTER_BOUND('',#2493,.T.);
#1728=FACE_OUTER_BOUND('',#2494,.T.);
#1729=FACE_OUTER_BOUND('',#2495,.T.);
#1730=FACE_OUTER_BOUND('',#2496,.T.);
#1731=FACE_OUTER_BOUND('',#2497,.T.);
#1732=FACE_OUTER_BOUND('',#2498,.T.);
#1733=FACE_OUTER_BOUND('',#2499,.T.);
#1734=FACE_OUTER_BOUND('',#2500,.T.);
#1735=FACE_OUTER_BOUND('',#2502,.T.);
#1736=FACE_OUTER_BOUND('',#2503,.T.);
#1737=FACE_OUTER_BOUND('',#2505,.T.);
#1738=FACE_OUTER_BOUND('',#2506,.T.);
#1739=FACE_OUTER_BOUND('',#2507,.T.);
#1740=FACE_OUTER_BOUND('',#2508,.T.);
#1741=FACE_OUTER_BOUND('',#2509,.T.);
#1742=FACE_OUTER_BOUND('',#2510,.T.);
#1743=FACE_OUTER_BOUND('',#2511,.T.);
#1744=FACE_OUTER_BOUND('',#2512,.T.);
#1745=FACE_OUTER_BOUND('',#2513,.T.);
#1746=FACE_OUTER_BOUND('',#2514,.T.);
#1747=FACE_OUTER_BOUND('',#2515,.T.);
#1748=FACE_OUTER_BOUND('',#2522,.T.);
#1749=FACE_OUTER_BOUND('',#2529,.T.);
#1750=FACE_OUTER_BOUND('',#2530,.T.);
#1751=FACE_OUTER_BOUND('',#2531,.T.);
#1752=FACE_OUTER_BOUND('',#2532,.T.);
#1753=FACE_OUTER_BOUND('',#2533,.T.);
#1754=FACE_OUTER_BOUND('',#2534,.T.);
#1755=FACE_OUTER_BOUND('',#2535,.T.);
#1756=FACE_OUTER_BOUND('',#2536,.T.);
#1757=FACE_OUTER_BOUND('',#2537,.T.);
#1758=FACE_OUTER_BOUND('',#2538,.T.);
#1759=FACE_OUTER_BOUND('',#2539,.T.);
#1760=FACE_OUTER_BOUND('',#2540,.T.);
#1761=FACE_OUTER_BOUND('',#2541,.T.);
#1762=FACE_OUTER_BOUND('',#2542,.T.);
#1763=FACE_OUTER_BOUND('',#2543,.T.);
#1764=FACE_OUTER_BOUND('',#2546,.T.);
#1765=FACE_OUTER_BOUND('',#2547,.T.);
#1766=FACE_OUTER_BOUND('',#2548,.T.);
#1767=FACE_OUTER_BOUND('',#2549,.T.);
#1768=FACE_OUTER_BOUND('',#2550,.T.);
#1769=FACE_OUTER_BOUND('',#2553,.T.);
#1770=FACE_OUTER_BOUND('',#2554,.T.);
#1771=FACE_OUTER_BOUND('',#2555,.T.);
#1772=FACE_OUTER_BOUND('',#2556,.T.);
#1773=FACE_OUTER_BOUND('',#2557,.T.);
#1774=FACE_OUTER_BOUND('',#2558,.T.);
#1775=FACE_OUTER_BOUND('',#2559,.T.);
#1776=FACE_OUTER_BOUND('',#2560,.T.);
#1777=FACE_OUTER_BOUND('',#2561,.T.);
#1778=FACE_OUTER_BOUND('',#2562,.T.);
#1779=FACE_OUTER_BOUND('',#2563,.T.);
#1780=FACE_OUTER_BOUND('',#2564,.T.);
#1781=FACE_OUTER_BOUND('',#2565,.T.);
#1782=FACE_OUTER_BOUND('',#2566,.T.);
#1783=FACE_OUTER_BOUND('',#2567,.T.);
#1784=FACE_OUTER_BOUND('',#2568,.T.);
#1785=FACE_OUTER_BOUND('',#2569,.T.);
#1786=FACE_OUTER_BOUND('',#2570,.T.);
#1787=FACE_OUTER_BOUND('',#2571,.T.);
#1788=FACE_OUTER_BOUND('',#2572,.T.);
#1789=FACE_OUTER_BOUND('',#2577,.T.);
#1790=FACE_OUTER_BOUND('',#2578,.T.);
#1791=FACE_OUTER_BOUND('',#2579,.T.);
#1792=FACE_OUTER_BOUND('',#2580,.T.);
#1793=FACE_OUTER_BOUND('',#2581,.T.);
#1794=FACE_OUTER_BOUND('',#2582,.T.);
#1795=FACE_OUTER_BOUND('',#2583,.T.);
#1796=FACE_OUTER_BOUND('',#2584,.T.);
#1797=FACE_OUTER_BOUND('',#2585,.T.);
#1798=FACE_OUTER_BOUND('',#2586,.T.);
#1799=FACE_OUTER_BOUND('',#2587,.T.);
#1800=FACE_OUTER_BOUND('',#2588,.T.);
#1801=FACE_OUTER_BOUND('',#2589,.T.);
#1802=FACE_OUTER_BOUND('',#2590,.T.);
#1803=FACE_OUTER_BOUND('',#2591,.T.);
#1804=FACE_OUTER_BOUND('',#2592,.T.);
#1805=FACE_OUTER_BOUND('',#2593,.T.);
#1806=FACE_OUTER_BOUND('',#2594,.T.);
#1807=FACE_OUTER_BOUND('',#2595,.T.);
#1808=FACE_OUTER_BOUND('',#2596,.T.);
#1809=FACE_OUTER_BOUND('',#2597,.T.);
#1810=FACE_OUTER_BOUND('',#2598,.T.);
#1811=FACE_OUTER_BOUND('',#2599,.T.);
#1812=FACE_OUTER_BOUND('',#2600,.T.);
#1813=FACE_OUTER_BOUND('',#2601,.T.);
#1814=FACE_OUTER_BOUND('',#2602,.T.);
#1815=FACE_OUTER_BOUND('',#2603,.T.);
#1816=FACE_OUTER_BOUND('',#2604,.T.);
#1817=FACE_OUTER_BOUND('',#2605,.T.);
#1818=FACE_OUTER_BOUND('',#2606,.T.);
#1819=FACE_OUTER_BOUND('',#2607,.T.);
#1820=FACE_OUTER_BOUND('',#2609,.T.);
#1821=FACE_OUTER_BOUND('',#2610,.T.);
#1822=FACE_OUTER_BOUND('',#2612,.T.);
#1823=FACE_OUTER_BOUND('',#2613,.T.);
#1824=FACE_OUTER_BOUND('',#2614,.T.);
#1825=FACE_OUTER_BOUND('',#2615,.T.);
#1826=FACE_OUTER_BOUND('',#2616,.T.);
#1827=FACE_OUTER_BOUND('',#2618,.T.);
#1828=FACE_OUTER_BOUND('',#2619,.T.);
#1829=FACE_OUTER_BOUND('',#2620,.T.);
#1830=FACE_OUTER_BOUND('',#2621,.T.);
#1831=FACE_OUTER_BOUND('',#2622,.T.);
#1832=FACE_OUTER_BOUND('',#2623,.T.);
#1833=FACE_OUTER_BOUND('',#2624,.T.);
#1834=FACE_OUTER_BOUND('',#2625,.T.);
#1835=FACE_OUTER_BOUND('',#2626,.T.);
#1836=FACE_OUTER_BOUND('',#2627,.T.);
#1837=FACE_OUTER_BOUND('',#2628,.T.);
#1838=FACE_OUTER_BOUND('',#2629,.T.);
#1839=FACE_OUTER_BOUND('',#2630,.T.);
#1840=FACE_OUTER_BOUND('',#2631,.T.);
#1841=FACE_OUTER_BOUND('',#2632,.T.);
#1842=FACE_OUTER_BOUND('',#2633,.T.);
#1843=FACE_OUTER_BOUND('',#2634,.T.);
#1844=FACE_OUTER_BOUND('',#2635,.T.);
#1845=FACE_OUTER_BOUND('',#2636,.T.);
#1846=FACE_OUTER_BOUND('',#2637,.T.);
#1847=FACE_OUTER_BOUND('',#2638,.T.);
#1848=FACE_OUTER_BOUND('',#2639,.T.);
#1849=FACE_OUTER_BOUND('',#2640,.T.);
#1850=FACE_OUTER_BOUND('',#2641,.T.);
#1851=FACE_OUTER_BOUND('',#2642,.T.);
#1852=FACE_OUTER_BOUND('',#2643,.T.);
#1853=FACE_OUTER_BOUND('',#2645,.T.);
#1854=FACE_OUTER_BOUND('',#2646,.T.);
#1855=FACE_OUTER_BOUND('',#2647,.T.);
#1856=FACE_OUTER_BOUND('',#2648,.T.);
#1857=FACE_OUTER_BOUND('',#2649,.T.);
#1858=FACE_OUTER_BOUND('',#2650,.T.);
#1859=FACE_OUTER_BOUND('',#2651,.T.);
#1860=FACE_OUTER_BOUND('',#2653,.T.);
#1861=FACE_OUTER_BOUND('',#2654,.T.);
#1862=FACE_OUTER_BOUND('',#2655,.T.);
#1863=FACE_OUTER_BOUND('',#2656,.T.);
#1864=FACE_OUTER_BOUND('',#2657,.T.);
#1865=FACE_OUTER_BOUND('',#2658,.T.);
#1866=FACE_OUTER_BOUND('',#2659,.T.);
#1867=FACE_OUTER_BOUND('',#2660,.T.);
#1868=FACE_OUTER_BOUND('',#2661,.T.);
#1869=FACE_OUTER_BOUND('',#2662,.T.);
#1870=FACE_OUTER_BOUND('',#2663,.T.);
#1871=FACE_OUTER_BOUND('',#2664,.T.);
#1872=EDGE_LOOP('',(#7253,#7254,#7255,#7256));
#1873=EDGE_LOOP('',(#7257));
#1874=EDGE_LOOP('',(#7258,#7259,#7260,#7261));
#1875=EDGE_LOOP('',(#7262));
#1876=EDGE_LOOP('',(#7263,#7264,#7265,#7266));
#1877=EDGE_LOOP('',(#7267));
#1878=EDGE_LOOP('',(#7268,#7269,#7270,#7271));
#1879=EDGE_LOOP('',(#7272));
#1880=EDGE_LOOP('',(#7273,#7274,#7275,#7276));
#1881=EDGE_LOOP('',(#7277));
#1882=EDGE_LOOP('',(#7278,#7279,#7280,#7281));
#1883=EDGE_LOOP('',(#7282));
#1884=EDGE_LOOP('',(#7283,#7284,#7285,#7286));
#1885=EDGE_LOOP('',(#7287));
#1886=EDGE_LOOP('',(#7288,#7289,#7290,#7291));
#1887=EDGE_LOOP('',(#7292));
#1888=EDGE_LOOP('',(#7293,#7294,#7295,#7296));
#1889=EDGE_LOOP('',(#7297,#7298,#7299,#7300));
#1890=EDGE_LOOP('',(#7301,#7302,#7303,#7304));
#1891=EDGE_LOOP('',(#7305,#7306,#7307,#7308));
#1892=EDGE_LOOP('',(#7309,#7310,#7311,#7312));
#1893=EDGE_LOOP('',(#7313));
#1894=EDGE_LOOP('',(#7314,#7315,#7316,#7317));
#1895=EDGE_LOOP('',(#7318));
#1896=EDGE_LOOP('',(#7319,#7320,#7321,#7322));
#1897=EDGE_LOOP('',(#7323));
#1898=EDGE_LOOP('',(#7324,#7325,#7326,#7327));
#1899=EDGE_LOOP('',(#7328));
#1900=EDGE_LOOP('',(#7329,#7330,#7331,#7332));
#1901=EDGE_LOOP('',(#7333));
#1902=EDGE_LOOP('',(#7334,#7335,#7336,#7337));
#1903=EDGE_LOOP('',(#7338));
#1904=EDGE_LOOP('',(#7339,#7340,#7341,#7342));
#1905=EDGE_LOOP('',(#7343));
#1906=EDGE_LOOP('',(#7344,#7345,#7346,#7347));
#1907=EDGE_LOOP('',(#7348));
#1908=EDGE_LOOP('',(#7349,#7350,#7351,#7352));
#1909=EDGE_LOOP('',(#7353,#7354,#7355,#7356));
#1910=EDGE_LOOP('',(#7357,#7358,#7359,#7360));
#1911=EDGE_LOOP('',(#7361,#7362,#7363,#7364));
#1912=EDGE_LOOP('',(#7365,#7366,#7367,#7368));
#1913=EDGE_LOOP('',(#7369));
#1914=EDGE_LOOP('',(#7370));
#1915=EDGE_LOOP('',(#7371));
#1916=EDGE_LOOP('',(#7372));
#1917=EDGE_LOOP('',(#7373));
#1918=EDGE_LOOP('',(#7374));
#1919=EDGE_LOOP('',(#7375));
#1920=EDGE_LOOP('',(#7376));
#1921=EDGE_LOOP('',(#7377));
#1922=EDGE_LOOP('',(#7378));
#1923=EDGE_LOOP('',(#7379));
#1924=EDGE_LOOP('',(#7380));
#1925=EDGE_LOOP('',(#7381));
#1926=EDGE_LOOP('',(#7382));
#1927=EDGE_LOOP('',(#7383));
#1928=EDGE_LOOP('',(#7384));
#1929=EDGE_LOOP('',(#7385));
#1930=EDGE_LOOP('',(#7386));
#1931=EDGE_LOOP('',(#7387));
#1932=EDGE_LOOP('',(#7388));
#1933=EDGE_LOOP('',(#7389,#7390,#7391,#7392));
#1934=EDGE_LOOP('',(#7393));
#1935=EDGE_LOOP('',(#7394));
#1936=EDGE_LOOP('',(#7395));
#1937=EDGE_LOOP('',(#7396));
#1938=EDGE_LOOP('',(#7397,#7398,#7399,#7400));
#1939=EDGE_LOOP('',(#7401,#7402,#7403,#7404));
#1940=EDGE_LOOP('',(#7405,#7406,#7407,#7408));
#1941=EDGE_LOOP('',(#7409,#7410,#7411,#7412));
#1942=EDGE_LOOP('',(#7413,#7414,#7415,#7416));
#1943=EDGE_LOOP('',(#7417,#7418,#7419,#7420));
#1944=EDGE_LOOP('',(#7421,#7422,#7423,#7424));
#1945=EDGE_LOOP('',(#7425,#7426,#7427,#7428));
#1946=EDGE_LOOP('',(#7429,#7430,#7431,#7432));
#1947=EDGE_LOOP('',(#7433,#7434,#7435,#7436));
#1948=EDGE_LOOP('',(#7437,#7438,#7439,#7440));
#1949=EDGE_LOOP('',(#7441,#7442,#7443,#7444));
#1950=EDGE_LOOP('',(#7445,#7446,#7447,#7448));
#1951=EDGE_LOOP('',(#7449,#7450,#7451,#7452));
#1952=EDGE_LOOP('',(#7453,#7454,#7455,#7456));
#1953=EDGE_LOOP('',(#7457,#7458,#7459,#7460));
#1954=EDGE_LOOP('',(#7461,#7462,#7463,#7464));
#1955=EDGE_LOOP('',(#7465,#7466,#7467,#7468));
#1956=EDGE_LOOP('',(#7469,#7470,#7471,#7472));
#1957=EDGE_LOOP('',(#7473,#7474,#7475,#7476));
#1958=EDGE_LOOP('',(#7477,#7478,#7479,#7480));
#1959=EDGE_LOOP('',(#7481,#7482,#7483,#7484));
#1960=EDGE_LOOP('',(#7485,#7486,#7487,#7488));
#1961=EDGE_LOOP('',(#7489,#7490,#7491,#7492));
#1962=EDGE_LOOP('',(#7493,#7494,#7495,#7496));
#1963=EDGE_LOOP('',(#7497,#7498,#7499,#7500));
#1964=EDGE_LOOP('',(#7501,#7502,#7503,#7504));
#1965=EDGE_LOOP('',(#7505,#7506,#7507,#7508));
#1966=EDGE_LOOP('',(#7509,#7510,#7511,#7512));
#1967=EDGE_LOOP('',(#7513,#7514,#7515,#7516));
#1968=EDGE_LOOP('',(#7517,#7518,#7519,#7520));
#1969=EDGE_LOOP('',(#7521,#7522,#7523,#7524));
#1970=EDGE_LOOP('',(#7525,#7526,#7527,#7528));
#1971=EDGE_LOOP('',(#7529,#7530,#7531,#7532));
#1972=EDGE_LOOP('',(#7533));
#1973=EDGE_LOOP('',(#7534));
#1974=EDGE_LOOP('',(#7535,#7536,#7537,#7538));
#1975=EDGE_LOOP('',(#7539));
#1976=EDGE_LOOP('',(#7540));
#1977=EDGE_LOOP('',(#7541,#7542,#7543,#7544));
#1978=EDGE_LOOP('',(#7545,#7546,#7547,#7548));
#1979=EDGE_LOOP('',(#7549,#7550,#7551,#7552,#7553,#7554,#7555,#7556));
#1980=EDGE_LOOP('',(#7557));
#1981=EDGE_LOOP('',(#7558));
#1982=EDGE_LOOP('',(#7559));
#1983=EDGE_LOOP('',(#7560));
#1984=EDGE_LOOP('',(#7561));
#1985=EDGE_LOOP('',(#7562,#7563,#7564,#7565));
#1986=EDGE_LOOP('',(#7566,#7567,#7568,#7569,#7570,#7571,#7572,#7573));
#1987=EDGE_LOOP('',(#7574));
#1988=EDGE_LOOP('',(#7575));
#1989=EDGE_LOOP('',(#7576));
#1990=EDGE_LOOP('',(#7577));
#1991=EDGE_LOOP('',(#7578));
#1992=EDGE_LOOP('',(#7579,#7580,#7581,#7582));
#1993=EDGE_LOOP('',(#7583,#7584,#7585,#7586));
#1994=EDGE_LOOP('',(#7587,#7588,#7589,#7590));
#1995=EDGE_LOOP('',(#7591));
#1996=EDGE_LOOP('',(#7592));
#1997=EDGE_LOOP('',(#7593));
#1998=EDGE_LOOP('',(#7594));
#1999=EDGE_LOOP('',(#7595,#7596,#7597,#7598));
#2000=EDGE_LOOP('',(#7599,#7600,#7601,#7602));
#2001=EDGE_LOOP('',(#7603));
#2002=EDGE_LOOP('',(#7604));
#2003=EDGE_LOOP('',(#7605));
#2004=EDGE_LOOP('',(#7606));
#2005=EDGE_LOOP('',(#7607,#7608,#7609,#7610));
#2006=EDGE_LOOP('',(#7611,#7612,#7613,#7614));
#2007=EDGE_LOOP('',(#7615,#7616,#7617,#7618));
#2008=EDGE_LOOP('',(#7619,#7620,#7621,#7622));
#2009=EDGE_LOOP('',(#7623,#7624,#7625,#7626,#7627,#7628,#7629,#7630));
#2010=EDGE_LOOP('',(#7631));
#2011=EDGE_LOOP('',(#7632,#7633,#7634,#7635));
#2012=EDGE_LOOP('',(#7636,#7637,#7638,#7639));
#2013=EDGE_LOOP('',(#7640,#7641,#7642,#7643));
#2014=EDGE_LOOP('',(#7644,#7645,#7646,#7647));
#2015=EDGE_LOOP('',(#7648,#7649,#7650,#7651));
#2016=EDGE_LOOP('',(#7652));
#2017=EDGE_LOOP('',(#7653));
#2018=EDGE_LOOP('',(#7654,#7655,#7656,#7657));
#2019=EDGE_LOOP('',(#7658,#7659,#7660,#7661,#7662,#7663,#7664,#7665));
#2020=EDGE_LOOP('',(#7666));
#2021=EDGE_LOOP('',(#7667,#7668,#7669,#7670));
#2022=EDGE_LOOP('',(#7671,#7672,#7673,#7674));
#2023=EDGE_LOOP('',(#7675,#7676,#7677,#7678));
#2024=EDGE_LOOP('',(#7679,#7680,#7681,#7682));
#2025=EDGE_LOOP('',(#7683,#7684,#7685,#7686,#7687,#7688,#7689,#7690));
#2026=EDGE_LOOP('',(#7691));
#2027=EDGE_LOOP('',(#7692,#7693,#7694,#7695));
#2028=EDGE_LOOP('',(#7696,#7697,#7698,#7699));
#2029=EDGE_LOOP('',(#7700,#7701,#7702,#7703));
#2030=EDGE_LOOP('',(#7704,#7705,#7706,#7707));
#2031=EDGE_LOOP('',(#7708,#7709,#7710,#7711));
#2032=EDGE_LOOP('',(#7712));
#2033=EDGE_LOOP('',(#7713));
#2034=EDGE_LOOP('',(#7714,#7715,#7716,#7717));
#2035=EDGE_LOOP('',(#7718,#7719,#7720,#7721,#7722,#7723,#7724,#7725));
#2036=EDGE_LOOP('',(#7726));
#2037=EDGE_LOOP('',(#7727,#7728,#7729,#7730));
#2038=EDGE_LOOP('',(#7731,#7732,#7733,#7734));
#2039=EDGE_LOOP('',(#7735,#7736,#7737,#7738));
#2040=EDGE_LOOP('',(#7739,#7740,#7741,#7742));
#2041=EDGE_LOOP('',(#7743,#7744,#7745,#7746));
#2042=EDGE_LOOP('',(#7747,#7748,#7749,#7750));
#2043=EDGE_LOOP('',(#7751,#7752,#7753,#7754));
#2044=EDGE_LOOP('',(#7755,#7756,#7757,#7758));
#2045=EDGE_LOOP('',(#7759,#7760,#7761,#7762));
#2046=EDGE_LOOP('',(#7763,#7764,#7765,#7766));
#2047=EDGE_LOOP('',(#7767));
#2048=EDGE_LOOP('',(#7768));
#2049=EDGE_LOOP('',(#7769,#7770,#7771,#7772));
#2050=EDGE_LOOP('',(#7773));
#2051=EDGE_LOOP('',(#7774));
#2052=EDGE_LOOP('',(#7775,#7776,#7777,#7778));
#2053=EDGE_LOOP('',(#7779,#7780,#7781,#7782));
#2054=EDGE_LOOP('',(#7783,#7784,#7785,#7786,#7787,#7788,#7789,#7790));
#2055=EDGE_LOOP('',(#7791));
#2056=EDGE_LOOP('',(#7792));
#2057=EDGE_LOOP('',(#7793));
#2058=EDGE_LOOP('',(#7794));
#2059=EDGE_LOOP('',(#7795));
#2060=EDGE_LOOP('',(#7796,#7797,#7798,#7799));
#2061=EDGE_LOOP('',(#7800,#7801,#7802,#7803,#7804,#7805,#7806,#7807));
#2062=EDGE_LOOP('',(#7808));
#2063=EDGE_LOOP('',(#7809));
#2064=EDGE_LOOP('',(#7810));
#2065=EDGE_LOOP('',(#7811));
#2066=EDGE_LOOP('',(#7812));
#2067=EDGE_LOOP('',(#7813,#7814,#7815,#7816));
#2068=EDGE_LOOP('',(#7817,#7818,#7819,#7820));
#2069=EDGE_LOOP('',(#7821,#7822,#7823,#7824));
#2070=EDGE_LOOP('',(#7825));
#2071=EDGE_LOOP('',(#7826));
#2072=EDGE_LOOP('',(#7827));
#2073=EDGE_LOOP('',(#7828));
#2074=EDGE_LOOP('',(#7829,#7830,#7831,#7832));
#2075=EDGE_LOOP('',(#7833,#7834,#7835,#7836));
#2076=EDGE_LOOP('',(#7837));
#2077=EDGE_LOOP('',(#7838));
#2078=EDGE_LOOP('',(#7839));
#2079=EDGE_LOOP('',(#7840));
#2080=EDGE_LOOP('',(#7841,#7842,#7843,#7844));
#2081=EDGE_LOOP('',(#7845,#7846,#7847,#7848));
#2082=EDGE_LOOP('',(#7849,#7850,#7851,#7852));
#2083=EDGE_LOOP('',(#7853,#7854,#7855,#7856));
#2084=EDGE_LOOP('',(#7857,#7858,#7859,#7860,#7861,#7862,#7863,#7864));
#2085=EDGE_LOOP('',(#7865));
#2086=EDGE_LOOP('',(#7866,#7867,#7868,#7869));
#2087=EDGE_LOOP('',(#7870,#7871,#7872,#7873));
#2088=EDGE_LOOP('',(#7874,#7875,#7876,#7877));
#2089=EDGE_LOOP('',(#7878,#7879,#7880,#7881));
#2090=EDGE_LOOP('',(#7882,#7883,#7884,#7885));
#2091=EDGE_LOOP('',(#7886));
#2092=EDGE_LOOP('',(#7887));
#2093=EDGE_LOOP('',(#7888,#7889,#7890,#7891));
#2094=EDGE_LOOP('',(#7892,#7893,#7894,#7895,#7896,#7897,#7898,#7899));
#2095=EDGE_LOOP('',(#7900));
#2096=EDGE_LOOP('',(#7901,#7902,#7903,#7904));
#2097=EDGE_LOOP('',(#7905,#7906,#7907,#7908));
#2098=EDGE_LOOP('',(#7909,#7910,#7911,#7912));
#2099=EDGE_LOOP('',(#7913,#7914,#7915,#7916));
#2100=EDGE_LOOP('',(#7917,#7918,#7919,#7920,#7921,#7922,#7923,#7924));
#2101=EDGE_LOOP('',(#7925));
#2102=EDGE_LOOP('',(#7926,#7927,#7928,#7929));
#2103=EDGE_LOOP('',(#7930,#7931,#7932,#7933));
#2104=EDGE_LOOP('',(#7934,#7935,#7936,#7937));
#2105=EDGE_LOOP('',(#7938,#7939,#7940,#7941));
#2106=EDGE_LOOP('',(#7942,#7943,#7944,#7945));
#2107=EDGE_LOOP('',(#7946));
#2108=EDGE_LOOP('',(#7947));
#2109=EDGE_LOOP('',(#7948,#7949,#7950,#7951));
#2110=EDGE_LOOP('',(#7952,#7953,#7954,#7955,#7956,#7957,#7958,#7959));
#2111=EDGE_LOOP('',(#7960));
#2112=EDGE_LOOP('',(#7961,#7962,#7963,#7964));
#2113=EDGE_LOOP('',(#7965,#7966,#7967,#7968));
#2114=EDGE_LOOP('',(#7969,#7970,#7971,#7972));
#2115=EDGE_LOOP('',(#7973,#7974,#7975,#7976));
#2116=EDGE_LOOP('',(#7977,#7978,#7979,#7980));
#2117=EDGE_LOOP('',(#7981,#7982,#7983,#7984));
#2118=EDGE_LOOP('',(#7985,#7986,#7987,#7988));
#2119=EDGE_LOOP('',(#7989,#7990,#7991,#7992));
#2120=EDGE_LOOP('',(#7993,#7994,#7995,#7996));
#2121=EDGE_LOOP('',(#7997,#7998,#7999,#8000));
#2122=EDGE_LOOP('',(#8001,#8002,#8003,#8004));
#2123=EDGE_LOOP('',(#8005,#8006,#8007,#8008));
#2124=EDGE_LOOP('',(#8009,#8010,#8011,#8012));
#2125=EDGE_LOOP('',(#8013,#8014,#8015,#8016));
#2126=EDGE_LOOP('',(#8017,#8018,#8019,#8020));
#2127=EDGE_LOOP('',(#8021));
#2128=EDGE_LOOP('',(#8022,#8023,#8024,#8025));
#2129=EDGE_LOOP('',(#8026,#8027,#8028,#8029));
#2130=EDGE_LOOP('',(#8030,#8031,#8032,#8033));
#2131=EDGE_LOOP('',(#8034));
#2132=EDGE_LOOP('',(#8035,#8036,#8037,#8038,#8039,#8040,#8041,#8042,#8043,
#8044,#8045,#8046,#8047,#8048,#8049,#8050));
#2133=EDGE_LOOP('',(#8051,#8052,#8053,#8054));
#2134=EDGE_LOOP('',(#8055,#8056,#8057,#8058));
#2135=EDGE_LOOP('',(#8059,#8060,#8061,#8062));
#2136=EDGE_LOOP('',(#8063,#8064,#8065,#8066));
#2137=EDGE_LOOP('',(#8067,#8068,#8069,#8070));
#2138=EDGE_LOOP('',(#8071,#8072,#8073,#8074));
#2139=EDGE_LOOP('',(#8075,#8076,#8077,#8078));
#2140=EDGE_LOOP('',(#8079,#8080,#8081,#8082));
#2141=EDGE_LOOP('',(#8083,#8084,#8085,#8086,#8087,#8088,#8089,#8090,#8091,
#8092,#8093,#8094,#8095,#8096,#8097,#8098));
#2142=EDGE_LOOP('',(#8099,#8100,#8101,#8102));
#2143=EDGE_LOOP('',(#8103));
#2144=EDGE_LOOP('',(#8104,#8105,#8106,#8107));
#2145=EDGE_LOOP('',(#8108));
#2146=EDGE_LOOP('',(#8109,#8110,#8111,#8112));
#2147=EDGE_LOOP('',(#8113,#8114,#8115,#8116));
#2148=EDGE_LOOP('',(#8117,#8118,#8119,#8120));
#2149=EDGE_LOOP('',(#8121,#8122,#8123,#8124));
#2150=EDGE_LOOP('',(#8125,#8126,#8127,#8128));
#2151=EDGE_LOOP('',(#8129));
#2152=EDGE_LOOP('',(#8130,#8131,#8132,#8133));
#2153=EDGE_LOOP('',(#8134,#8135,#8136,#8137));
#2154=EDGE_LOOP('',(#8138,#8139,#8140,#8141));
#2155=EDGE_LOOP('',(#8142));
#2156=EDGE_LOOP('',(#8143,#8144,#8145,#8146,#8147,#8148,#8149,#8150,#8151,
#8152,#8153,#8154,#8155,#8156,#8157,#8158));
#2157=EDGE_LOOP('',(#8159,#8160,#8161,#8162));
#2158=EDGE_LOOP('',(#8163,#8164,#8165,#8166));
#2159=EDGE_LOOP('',(#8167,#8168,#8169,#8170));
#2160=EDGE_LOOP('',(#8171,#8172,#8173,#8174));
#2161=EDGE_LOOP('',(#8175,#8176,#8177,#8178));
#2162=EDGE_LOOP('',(#8179,#8180,#8181,#8182));
#2163=EDGE_LOOP('',(#8183,#8184,#8185,#8186));
#2164=EDGE_LOOP('',(#8187,#8188,#8189,#8190));
#2165=EDGE_LOOP('',(#8191,#8192,#8193,#8194,#8195,#8196,#8197,#8198,#8199,
#8200,#8201,#8202,#8203,#8204,#8205,#8206));
#2166=EDGE_LOOP('',(#8207,#8208,#8209,#8210));
#2167=EDGE_LOOP('',(#8211));
#2168=EDGE_LOOP('',(#8212,#8213,#8214,#8215));
#2169=EDGE_LOOP('',(#8216));
#2170=EDGE_LOOP('',(#8217,#8218,#8219,#8220));
#2171=EDGE_LOOP('',(#8221,#8222,#8223,#8224));
#2172=EDGE_LOOP('',(#8225,#8226,#8227,#8228,#8229,#8230));
#2173=EDGE_LOOP('',(#8231,#8232,#8233,#8234,#8235));
#2174=EDGE_LOOP('',(#8236,#8237,#8238,#8239));
#2175=EDGE_LOOP('',(#8240,#8241,#8242,#8243));
#2176=EDGE_LOOP('',(#8244));
#2177=EDGE_LOOP('',(#8245));
#2178=EDGE_LOOP('',(#8246,#8247,#8248,#8249,#8250));
#2179=EDGE_LOOP('',(#8251));
#2180=EDGE_LOOP('',(#8252));
#2181=EDGE_LOOP('',(#8253,#8254,#8255,#8256));
#2182=EDGE_LOOP('',(#8257,#8258,#8259,#8260,#8261,#8262));
#2183=EDGE_LOOP('',(#8263,#8264,#8265,#8266,#8267));
#2184=EDGE_LOOP('',(#8268));
#2185=EDGE_LOOP('',(#8269));
#2186=EDGE_LOOP('',(#8270,#8271,#8272,#8273));
#2187=EDGE_LOOP('',(#8274,#8275,#8276,#8277));
#2188=EDGE_LOOP('',(#8278,#8279,#8280,#8281));
#2189=EDGE_LOOP('',(#8282));
#2190=EDGE_LOOP('',(#8283));
#2191=EDGE_LOOP('',(#8284,#8285,#8286,#8287,#8288));
#2192=EDGE_LOOP('',(#8289,#8290));
#2193=EDGE_LOOP('',(#8291,#8292));
#2194=EDGE_LOOP('',(#8293,#8294));
#2195=EDGE_LOOP('',(#8295,#8296));
#2196=EDGE_LOOP('',(#8297,#8298));
#2197=EDGE_LOOP('',(#8299,#8300));
#2198=EDGE_LOOP('',(#8301,#8302));
#2199=EDGE_LOOP('',(#8303,#8304));
#2200=EDGE_LOOP('',(#8305,#8306,#8307,#8308));
#2201=EDGE_LOOP('',(#8309,#8310,#8311,#8312,#8313,#8314,#8315,#8316,#8317,
#8318,#8319,#8320,#8321,#8322,#8323,#8324,#8325,#8326,#8327,#8328));
#2202=EDGE_LOOP('',(#8329,#8330,#8331,#8332));
#2203=EDGE_LOOP('',(#8333,#8334,#8335,#8336));
#2204=EDGE_LOOP('',(#8337,#8338,#8339,#8340));
#2205=EDGE_LOOP('',(#8341,#8342,#8343,#8344));
#2206=EDGE_LOOP('',(#8345,#8346,#8347,#8348));
#2207=EDGE_LOOP('',(#8349,#8350,#8351,#8352,#8353,#8354));
#2208=EDGE_LOOP('',(#8355,#8356,#8357,#8358));
#2209=EDGE_LOOP('',(#8359,#8360,#8361,#8362));
#2210=EDGE_LOOP('',(#8363,#8364,#8365,#8366));
#2211=EDGE_LOOP('',(#8367,#8368,#8369,#8370));
#2212=EDGE_LOOP('',(#8371,#8372,#8373,#8374));
#2213=EDGE_LOOP('',(#8375,#8376,#8377,#8378));
#2214=EDGE_LOOP('',(#8379,#8380,#8381,#8382,#8383,#8384,#8385,#8386,#8387,
#8388,#8389,#8390,#8391,#8392,#8393,#8394,#8395,#8396,#8397,#8398));
#2215=EDGE_LOOP('',(#8399,#8400,#8401,#8402));
#2216=EDGE_LOOP('',(#8403,#8404,#8405,#8406));
#2217=EDGE_LOOP('',(#8407));
#2218=EDGE_LOOP('',(#8408));
#2219=EDGE_LOOP('',(#8409,#8410,#8411,#8412));
#2220=EDGE_LOOP('',(#8413));
#2221=EDGE_LOOP('',(#8414));
#2222=EDGE_LOOP('',(#8415,#8416,#8417,#8418));
#2223=EDGE_LOOP('',(#8419));
#2224=EDGE_LOOP('',(#8420));
#2225=EDGE_LOOP('',(#8421,#8422,#8423,#8424));
#2226=EDGE_LOOP('',(#8425));
#2227=EDGE_LOOP('',(#8426));
#2228=EDGE_LOOP('',(#8427,#8428,#8429,#8430));
#2229=EDGE_LOOP('',(#8431));
#2230=EDGE_LOOP('',(#8432));
#2231=EDGE_LOOP('',(#8433,#8434,#8435,#8436));
#2232=EDGE_LOOP('',(#8437,#8438,#8439,#8440));
#2233=EDGE_LOOP('',(#8441,#8442,#8443,#8444));
#2234=EDGE_LOOP('',(#8445,#8446,#8447,#8448));
#2235=EDGE_LOOP('',(#8449,#8450,#8451,#8452));
#2236=EDGE_LOOP('',(#8453,#8454,#8455,#8456));
#2237=EDGE_LOOP('',(#8457,#8458,#8459,#8460));
#2238=EDGE_LOOP('',(#8461,#8462,#8463,#8464));
#2239=EDGE_LOOP('',(#8465,#8466,#8467,#8468));
#2240=EDGE_LOOP('',(#8469,#8470,#8471,#8472));
#2241=EDGE_LOOP('',(#8473,#8474,#8475,#8476));
#2242=EDGE_LOOP('',(#8477,#8478,#8479,#8480));
#2243=EDGE_LOOP('',(#8481,#8482,#8483,#8484));
#2244=EDGE_LOOP('',(#8485,#8486,#8487,#8488));
#2245=EDGE_LOOP('',(#8489,#8490,#8491,#8492));
#2246=EDGE_LOOP('',(#8493,#8494,#8495,#8496));
#2247=EDGE_LOOP('',(#8497,#8498,#8499,#8500));
#2248=EDGE_LOOP('',(#8501,#8502,#8503,#8504));
#2249=EDGE_LOOP('',(#8505,#8506,#8507,#8508));
#2250=EDGE_LOOP('',(#8509,#8510,#8511,#8512));
#2251=EDGE_LOOP('',(#8513,#8514,#8515,#8516));
#2252=EDGE_LOOP('',(#8517,#8518,#8519,#8520));
#2253=EDGE_LOOP('',(#8521,#8522,#8523,#8524));
#2254=EDGE_LOOP('',(#8525,#8526,#8527,#8528));
#2255=EDGE_LOOP('',(#8529,#8530,#8531,#8532));
#2256=EDGE_LOOP('',(#8533,#8534,#8535,#8536));
#2257=EDGE_LOOP('',(#8537,#8538,#8539,#8540));
#2258=EDGE_LOOP('',(#8541,#8542,#8543,#8544));
#2259=EDGE_LOOP('',(#8545,#8546,#8547,#8548));
#2260=EDGE_LOOP('',(#8549,#8550,#8551,#8552));
#2261=EDGE_LOOP('',(#8553,#8554,#8555,#8556));
#2262=EDGE_LOOP('',(#8557,#8558,#8559,#8560));
#2263=EDGE_LOOP('',(#8561,#8562,#8563,#8564));
#2264=EDGE_LOOP('',(#8565,#8566,#8567,#8568));
#2265=EDGE_LOOP('',(#8569,#8570,#8571,#8572));
#2266=EDGE_LOOP('',(#8573,#8574,#8575,#8576));
#2267=EDGE_LOOP('',(#8577,#8578,#8579,#8580));
#2268=EDGE_LOOP('',(#8581,#8582,#8583,#8584));
#2269=EDGE_LOOP('',(#8585,#8586,#8587,#8588));
#2270=EDGE_LOOP('',(#8589,#8590,#8591,#8592));
#2271=EDGE_LOOP('',(#8593,#8594,#8595,#8596));
#2272=EDGE_LOOP('',(#8597,#8598,#8599,#8600));
#2273=EDGE_LOOP('',(#8601,#8602,#8603,#8604));
#2274=EDGE_LOOP('',(#8605,#8606,#8607,#8608));
#2275=EDGE_LOOP('',(#8609,#8610,#8611,#8612));
#2276=EDGE_LOOP('',(#8613,#8614,#8615,#8616));
#2277=EDGE_LOOP('',(#8617,#8618,#8619,#8620,#8621,#8622,#8623,#8624,#8625,
#8626,#8627,#8628,#8629,#8630,#8631,#8632,#8633,#8634,#8635,#8636,#8637,
#8638,#8639,#8640,#8641,#8642,#8643,#8644,#8645,#8646,#8647,#8648,#8649,
#8650,#8651,#8652,#8653,#8654,#8655,#8656,#8657,#8658,#8659,#8660));
#2278=EDGE_LOOP('',(#8661));
#2279=EDGE_LOOP('',(#8662,#8663,#8664,#8665,#8666,#8667,#8668,#8669,#8670,
#8671,#8672,#8673,#8674,#8675,#8676,#8677,#8678,#8679,#8680,#8681,#8682,
#8683,#8684,#8685,#8686,#8687,#8688,#8689,#8690,#8691,#8692,#8693,#8694,
#8695,#8696,#8697,#8698,#8699,#8700,#8701,#8702,#8703,#8704,#8705));
#2280=EDGE_LOOP('',(#8706));
#2281=EDGE_LOOP('',(#8707,#8708,#8709,#8710));
#2282=EDGE_LOOP('',(#8711,#8712,#8713,#8714));
#2283=EDGE_LOOP('',(#8715,#8716,#8717,#8718));
#2284=EDGE_LOOP('',(#8719));
#2285=EDGE_LOOP('',(#8720,#8721,#8722,#8723,#8724,#8725,#8726,#8727,#8728,
#8729));
#2286=EDGE_LOOP('',(#8730,#8731,#8732,#8733));
#2287=EDGE_LOOP('',(#8734,#8735,#8736,#8737));
#2288=EDGE_LOOP('',(#8738,#8739,#8740,#8741,#8742,#8743,#8744,#8745,#8746,
#8747));
#2289=EDGE_LOOP('',(#8748,#8749,#8750,#8751));
#2290=EDGE_LOOP('',(#8752,#8753,#8754,#8755,#8756,#8757));
#2291=EDGE_LOOP('',(#8758,#8759,#8760,#8761,#8762,#8763,#8764,#8765));
#2292=EDGE_LOOP('',(#8766,#8767,#8768,#8769,#8770));
#2293=EDGE_LOOP('',(#8771,#8772,#8773,#8774));
#2294=EDGE_LOOP('',(#8775,#8776,#8777,#8778,#8779,#8780));
#2295=EDGE_LOOP('',(#8781,#8782,#8783,#8784));
#2296=EDGE_LOOP('',(#8785,#8786,#8787,#8788));
#2297=EDGE_LOOP('',(#8789,#8790,#8791,#8792));
#2298=EDGE_LOOP('',(#8793,#8794,#8795,#8796));
#2299=EDGE_LOOP('',(#8797,#8798,#8799,#8800));
#2300=EDGE_LOOP('',(#8801,#8802,#8803,#8804));
#2301=EDGE_LOOP('',(#8805,#8806,#8807,#8808));
#2302=EDGE_LOOP('',(#8809,#8810,#8811,#8812,#8813,#8814));
#2303=EDGE_LOOP('',(#8815,#8816,#8817,#8818,#8819,#8820));
#2304=EDGE_LOOP('',(#8821));
#2305=EDGE_LOOP('',(#8822));
#2306=EDGE_LOOP('',(#8823,#8824,#8825,#8826));
#2307=EDGE_LOOP('',(#8827,#8828,#8829,#8830));
#2308=EDGE_LOOP('',(#8831,#8832,#8833,#8834));
#2309=EDGE_LOOP('',(#8835));
#2310=EDGE_LOOP('',(#8836));
#2311=EDGE_LOOP('',(#8837,#8838,#8839,#8840));
#2312=EDGE_LOOP('',(#8841,#8842,#8843,#8844));
#2313=EDGE_LOOP('',(#8845,#8846,#8847,#8848));
#2314=EDGE_LOOP('',(#8849));
#2315=EDGE_LOOP('',(#8850));
#2316=EDGE_LOOP('',(#8851,#8852,#8853,#8854));
#2317=EDGE_LOOP('',(#8855));
#2318=EDGE_LOOP('',(#8856));
#2319=EDGE_LOOP('',(#8857,#8858,#8859,#8860));
#2320=EDGE_LOOP('',(#8861));
#2321=EDGE_LOOP('',(#8862));
#2322=EDGE_LOOP('',(#8863,#8864,#8865,#8866));
#2323=EDGE_LOOP('',(#8867));
#2324=EDGE_LOOP('',(#8868));
#2325=EDGE_LOOP('',(#8869,#8870,#8871,#8872));
#2326=EDGE_LOOP('',(#8873,#8874,#8875,#8876));
#2327=EDGE_LOOP('',(#8877,#8878,#8879,#8880));
#2328=EDGE_LOOP('',(#8881,#8882,#8883,#8884));
#2329=EDGE_LOOP('',(#8885,#8886,#8887,#8888));
#2330=EDGE_LOOP('',(#8889,#8890,#8891,#8892));
#2331=EDGE_LOOP('',(#8893,#8894,#8895,#8896));
#2332=EDGE_LOOP('',(#8897,#8898,#8899,#8900));
#2333=EDGE_LOOP('',(#8901,#8902,#8903,#8904));
#2334=EDGE_LOOP('',(#8905));
#2335=EDGE_LOOP('',(#8906));
#2336=EDGE_LOOP('',(#8907));
#2337=EDGE_LOOP('',(#8908));
#2338=EDGE_LOOP('',(#8909,#8910,#8911,#8912));
#2339=EDGE_LOOP('',(#8913,#8914,#8915,#8916));
#2340=EDGE_LOOP('',(#8917,#8918,#8919,#8920));
#2341=EDGE_LOOP('',(#8921,#8922,#8923,#8924));
#2342=EDGE_LOOP('',(#8925,#8926,#8927,#8928));
#2343=EDGE_LOOP('',(#8929,#8930,#8931,#8932));
#2344=EDGE_LOOP('',(#8933));
#2345=EDGE_LOOP('',(#8934));
#2346=EDGE_LOOP('',(#8935));
#2347=EDGE_LOOP('',(#8936));
#2348=EDGE_LOOP('',(#8937,#8938,#8939,#8940));
#2349=EDGE_LOOP('',(#8941,#8942,#8943,#8944,#8945,#8946,#8947,#8948,#8949,
#8950,#8951,#8952));
#2350=EDGE_LOOP('',(#8953,#8954,#8955,#8956,#8957,#8958,#8959,#8960,#8961,
#8962,#8963,#8964));
#2351=EDGE_LOOP('',(#8965,#8966,#8967,#8968));
#2352=EDGE_LOOP('',(#8969));
#2353=EDGE_LOOP('',(#8970));
#2354=EDGE_LOOP('',(#8971));
#2355=EDGE_LOOP('',(#8972));
#2356=EDGE_LOOP('',(#8973));
#2357=EDGE_LOOP('',(#8974,#8975,#8976,#8977));
#2358=EDGE_LOOP('',(#8978,#8979,#8980,#8981));
#2359=EDGE_LOOP('',(#8982,#8983,#8984,#8985));
#2360=EDGE_LOOP('',(#8986));
#2361=EDGE_LOOP('',(#8987));
#2362=EDGE_LOOP('',(#8988,#8989,#8990,#8991));
#2363=EDGE_LOOP('',(#8992));
#2364=EDGE_LOOP('',(#8993));
#2365=EDGE_LOOP('',(#8994));
#2366=EDGE_LOOP('',(#8995,#8996,#8997,#8998));
#2367=EDGE_LOOP('',(#8999));
#2368=EDGE_LOOP('',(#9000));
#2369=EDGE_LOOP('',(#9001,#9002,#9003,#9004));
#2370=EDGE_LOOP('',(#9005,#9006,#9007,#9008));
#2371=EDGE_LOOP('',(#9009));
#2372=EDGE_LOOP('',(#9010));
#2373=EDGE_LOOP('',(#9011));
#2374=EDGE_LOOP('',(#9012));
#2375=EDGE_LOOP('',(#9013,#9014,#9015,#9016));
#2376=EDGE_LOOP('',(#9017,#9018,#9019,#9020));
#2377=EDGE_LOOP('',(#9021));
#2378=EDGE_LOOP('',(#9022));
#2379=EDGE_LOOP('',(#9023));
#2380=EDGE_LOOP('',(#9024));
#2381=EDGE_LOOP('',(#9025,#9026,#9027,#9028));
#2382=EDGE_LOOP('',(#9029));
#2383=EDGE_LOOP('',(#9030));
#2384=EDGE_LOOP('',(#9031,#9032,#9033,#9034));
#2385=EDGE_LOOP('',(#9035));
#2386=EDGE_LOOP('',(#9036));
#2387=EDGE_LOOP('',(#9037,#9038,#9039,#9040));
#2388=EDGE_LOOP('',(#9041,#9042,#9043,#9044));
#2389=EDGE_LOOP('',(#9045));
#2390=EDGE_LOOP('',(#9046));
#2391=EDGE_LOOP('',(#9047));
#2392=EDGE_LOOP('',(#9048));
#2393=EDGE_LOOP('',(#9049,#9050,#9051,#9052));
#2394=EDGE_LOOP('',(#9053));
#2395=EDGE_LOOP('',(#9054));
#2396=EDGE_LOOP('',(#9055));
#2397=EDGE_LOOP('',(#9056));
#2398=EDGE_LOOP('',(#9057));
#2399=EDGE_LOOP('',(#9058,#9059,#9060,#9061));
#2400=EDGE_LOOP('',(#9062,#9063,#9064,#9065));
#2401=EDGE_LOOP('',(#9066,#9067,#9068,#9069));
#2402=EDGE_LOOP('',(#9070));
#2403=EDGE_LOOP('',(#9071));
#2404=EDGE_LOOP('',(#9072,#9073,#9074,#9075));
#2405=EDGE_LOOP('',(#9076));
#2406=EDGE_LOOP('',(#9077));
#2407=EDGE_LOOP('',(#9078));
#2408=EDGE_LOOP('',(#9079,#9080,#9081,#9082));
#2409=EDGE_LOOP('',(#9083));
#2410=EDGE_LOOP('',(#9084));
#2411=EDGE_LOOP('',(#9085,#9086,#9087,#9088));
#2412=EDGE_LOOP('',(#9089,#9090,#9091,#9092));
#2413=EDGE_LOOP('',(#9093));
#2414=EDGE_LOOP('',(#9094));
#2415=EDGE_LOOP('',(#9095));
#2416=EDGE_LOOP('',(#9096));
#2417=EDGE_LOOP('',(#9097,#9098,#9099,#9100));
#2418=EDGE_LOOP('',(#9101,#9102,#9103,#9104));
#2419=EDGE_LOOP('',(#9105));
#2420=EDGE_LOOP('',(#9106));
#2421=EDGE_LOOP('',(#9107));
#2422=EDGE_LOOP('',(#9108));
#2423=EDGE_LOOP('',(#9109,#9110,#9111,#9112));
#2424=EDGE_LOOP('',(#9113));
#2425=EDGE_LOOP('',(#9114));
#2426=EDGE_LOOP('',(#9115,#9116,#9117,#9118));
#2427=EDGE_LOOP('',(#9119));
#2428=EDGE_LOOP('',(#9120));
#2429=EDGE_LOOP('',(#9121,#9122,#9123,#9124));
#2430=EDGE_LOOP('',(#9125,#9126,#9127,#9128));
#2431=EDGE_LOOP('',(#9129));
#2432=EDGE_LOOP('',(#9130));
#2433=EDGE_LOOP('',(#9131));
#2434=EDGE_LOOP('',(#9132));
#2435=EDGE_LOOP('',(#9133,#9134,#9135,#9136,#9137,#9138,#9139,#9140,#9141));
#2436=EDGE_LOOP('',(#9142,#9143,#9144,#9145,#9146,#9147,#9148));
#2437=EDGE_LOOP('',(#9149,#9150,#9151,#9152,#9153,#9154,#9155,#9156,#9157));
#2438=EDGE_LOOP('',(#9158,#9159,#9160));
#2439=EDGE_LOOP('',(#9161,#9162,#9163));
#2440=EDGE_LOOP('',(#9164,#9165,#9166));
#2441=EDGE_LOOP('',(#9167,#9168,#9169,#9170,#9171,#9172,#9173));
#2442=EDGE_LOOP('',(#9174,#9175,#9176,#9177,#9178,#9179,#9180));
#2443=EDGE_LOOP('',(#9181,#9182,#9183,#9184,#9185,#9186,#9187,#9188,#9189,
#9190));
#2444=EDGE_LOOP('',(#9191,#9192));
#2445=EDGE_LOOP('',(#9193,#9194));
#2446=EDGE_LOOP('',(#9195,#9196));
#2447=EDGE_LOOP('',(#9197));
#2448=EDGE_LOOP('',(#9198));
#2449=EDGE_LOOP('',(#9199));
#2450=EDGE_LOOP('',(#9200,#9201,#9202,#9203,#9204,#9205,#9206,#9207,#9208,
#9209,#9210,#9211,#9212,#9213,#9214,#9215,#9216,#9217,#9218,#9219,#9220,
#9221,#9222,#9223,#9224,#9225,#9226,#9227,#9228,#9229,#9230,#9231,#9232,
#9233,#9234,#9235,#9236,#9237,#9238,#9239));
#2451=EDGE_LOOP('',(#9240,#9241,#9242,#9243));
#2452=EDGE_LOOP('',(#9244));
#2453=EDGE_LOOP('',(#9245));
#2454=EDGE_LOOP('',(#9246));
#2455=EDGE_LOOP('',(#9247,#9248,#9249,#9250,#9251,#9252,#9253,#9254,#9255,
#9256,#9257,#9258,#9259,#9260,#9261,#9262,#9263,#9264,#9265,#9266,#9267,
#9268,#9269,#9270,#9271,#9272,#9273,#9274,#9275,#9276,#9277,#9278,#9279,
#9280,#9281,#9282,#9283,#9284,#9285,#9286));
#2456=EDGE_LOOP('',(#9287,#9288,#9289,#9290));
#2457=EDGE_LOOP('',(#9291));
#2458=EDGE_LOOP('',(#9292));
#2459=EDGE_LOOP('',(#9293,#9294,#9295,#9296));
#2460=EDGE_LOOP('',(#9297,#9298,#9299,#9300));
#2461=EDGE_LOOP('',(#9301,#9302,#9303,#9304));
#2462=EDGE_LOOP('',(#9305,#9306,#9307,#9308));
#2463=EDGE_LOOP('',(#9309,#9310,#9311,#9312));
#2464=EDGE_LOOP('',(#9313,#9314,#9315,#9316));
#2465=EDGE_LOOP('',(#9317,#9318,#9319,#9320));
#2466=EDGE_LOOP('',(#9321,#9322,#9323,#9324));
#2467=EDGE_LOOP('',(#9325,#9326,#9327,#9328));
#2468=EDGE_LOOP('',(#9329,#9330,#9331,#9332));
#2469=EDGE_LOOP('',(#9333,#9334,#9335,#9336));
#2470=EDGE_LOOP('',(#9337,#9338,#9339,#9340));
#2471=EDGE_LOOP('',(#9341,#9342,#9343,#9344));
#2472=EDGE_LOOP('',(#9345,#9346,#9347,#9348));
#2473=EDGE_LOOP('',(#9349,#9350,#9351,#9352));
#2474=EDGE_LOOP('',(#9353,#9354,#9355,#9356));
#2475=EDGE_LOOP('',(#9357,#9358,#9359,#9360));
#2476=EDGE_LOOP('',(#9361,#9362,#9363,#9364));
#2477=EDGE_LOOP('',(#9365,#9366,#9367,#9368));
#2478=EDGE_LOOP('',(#9369,#9370,#9371,#9372));
#2479=EDGE_LOOP('',(#9373,#9374,#9375,#9376));
#2480=EDGE_LOOP('',(#9377,#9378,#9379,#9380));
#2481=EDGE_LOOP('',(#9381,#9382,#9383,#9384));
#2482=EDGE_LOOP('',(#9385,#9386,#9387,#9388));
#2483=EDGE_LOOP('',(#9389,#9390,#9391,#9392));
#2484=EDGE_LOOP('',(#9393,#9394,#9395,#9396));
#2485=EDGE_LOOP('',(#9397,#9398,#9399,#9400));
#2486=EDGE_LOOP('',(#9401,#9402,#9403,#9404));
#2487=EDGE_LOOP('',(#9405,#9406,#9407,#9408));
#2488=EDGE_LOOP('',(#9409,#9410,#9411,#9412));
#2489=EDGE_LOOP('',(#9413,#9414,#9415,#9416));
#2490=EDGE_LOOP('',(#9417,#9418,#9419,#9420));
#2491=EDGE_LOOP('',(#9421,#9422,#9423,#9424));
#2492=EDGE_LOOP('',(#9425,#9426,#9427,#9428));
#2493=EDGE_LOOP('',(#9429,#9430,#9431,#9432));
#2494=EDGE_LOOP('',(#9433,#9434,#9435,#9436));
#2495=EDGE_LOOP('',(#9437,#9438,#9439,#9440));
#2496=EDGE_LOOP('',(#9441,#9442,#9443,#9444));
#2497=EDGE_LOOP('',(#9445,#9446,#9447,#9448));
#2498=EDGE_LOOP('',(#9449,#9450,#9451,#9452));
#2499=EDGE_LOOP('',(#9453,#9454,#9455,#9456));
#2500=EDGE_LOOP('',(#9457));
#2501=EDGE_LOOP('',(#9458));
#2502=EDGE_LOOP('',(#9459,#9460,#9461,#9462));
#2503=EDGE_LOOP('',(#9463));
#2504=EDGE_LOOP('',(#9464));
#2505=EDGE_LOOP('',(#9465,#9466,#9467,#9468));
#2506=EDGE_LOOP('',(#9469,#9470,#9471,#9472));
#2507=EDGE_LOOP('',(#9473,#9474,#9475,#9476));
#2508=EDGE_LOOP('',(#9477,#9478,#9479,#9480));
#2509=EDGE_LOOP('',(#9481,#9482,#9483,#9484));
#2510=EDGE_LOOP('',(#9485,#9486,#9487,#9488));
#2511=EDGE_LOOP('',(#9489,#9490,#9491,#9492));
#2512=EDGE_LOOP('',(#9493,#9494,#9495,#9496));
#2513=EDGE_LOOP('',(#9497,#9498,#9499,#9500));
#2514=EDGE_LOOP('',(#9501,#9502,#9503,#9504));
#2515=EDGE_LOOP('',(#9505,#9506,#9507,#9508));
#2516=EDGE_LOOP('',(#9509));
#2517=EDGE_LOOP('',(#9510));
#2518=EDGE_LOOP('',(#9511));
#2519=EDGE_LOOP('',(#9512));
#2520=EDGE_LOOP('',(#9513));
#2521=EDGE_LOOP('',(#9514));
#2522=EDGE_LOOP('',(#9515,#9516,#9517,#9518));
#2523=EDGE_LOOP('',(#9519));
#2524=EDGE_LOOP('',(#9520));
#2525=EDGE_LOOP('',(#9521));
#2526=EDGE_LOOP('',(#9522));
#2527=EDGE_LOOP('',(#9523));
#2528=EDGE_LOOP('',(#9524));
#2529=EDGE_LOOP('',(#9525,#9526,#9527,#9528));
#2530=EDGE_LOOP('',(#9529));
#2531=EDGE_LOOP('',(#9530,#9531,#9532,#9533));
#2532=EDGE_LOOP('',(#9534));
#2533=EDGE_LOOP('',(#9535,#9536,#9537,#9538));
#2534=EDGE_LOOP('',(#9539,#9540,#9541,#9542));
#2535=EDGE_LOOP('',(#9543,#9544,#9545,#9546));
#2536=EDGE_LOOP('',(#9547,#9548,#9549,#9550));
#2537=EDGE_LOOP('',(#9551,#9552,#9553,#9554,#9555,#9556));
#2538=EDGE_LOOP('',(#9557,#9558,#9559,#9560,#9561,#9562,#9563,#9564));
#2539=EDGE_LOOP('',(#9565,#9566,#9567,#9568));
#2540=EDGE_LOOP('',(#9569));
#2541=EDGE_LOOP('',(#9570,#9571,#9572,#9573));
#2542=EDGE_LOOP('',(#9574));
#2543=EDGE_LOOP('',(#9575,#9576,#9577,#9578));
#2544=EDGE_LOOP('',(#9579));
#2545=EDGE_LOOP('',(#9580));
#2546=EDGE_LOOP('',(#9581,#9582,#9583,#9584));
#2547=EDGE_LOOP('',(#9585,#9586,#9587,#9588));
#2548=EDGE_LOOP('',(#9589,#9590,#9591,#9592,#9593,#9594,#9595,#9596));
#2549=EDGE_LOOP('',(#9597,#9598,#9599,#9600,#9601,#9602));
#2550=EDGE_LOOP('',(#9603,#9604,#9605,#9606));
#2551=EDGE_LOOP('',(#9607));
#2552=EDGE_LOOP('',(#9608));
#2553=EDGE_LOOP('',(#9609,#9610,#9611,#9612));
#2554=EDGE_LOOP('',(#9613,#9614,#9615,#9616));
#2555=EDGE_LOOP('',(#9617,#9618,#9619,#9620));
#2556=EDGE_LOOP('',(#9621,#9622,#9623,#9624));
#2557=EDGE_LOOP('',(#9625,#9626,#9627,#9628));
#2558=EDGE_LOOP('',(#9629,#9630,#9631,#9632));
#2559=EDGE_LOOP('',(#9633,#9634));
#2560=EDGE_LOOP('',(#9635,#9636,#9637,#9638,#9639,#9640,#9641,#9642));
#2561=EDGE_LOOP('',(#9643,#9644));
#2562=EDGE_LOOP('',(#9645,#9646,#9647,#9648,#9649,#9650,#9651,#9652));
#2563=EDGE_LOOP('',(#9653,#9654));
#2564=EDGE_LOOP('',(#9655,#9656,#9657,#9658,#9659,#9660,#9661,#9662));
#2565=EDGE_LOOP('',(#9663,#9664));
#2566=EDGE_LOOP('',(#9665,#9666,#9667,#9668,#9669,#9670,#9671,#9672));
#2567=EDGE_LOOP('',(#9673,#9674,#9675,#9676,#9677,#9678,#9679,#9680,#9681,
#9682,#9683,#9684));
#2568=EDGE_LOOP('',(#9685,#9686,#9687,#9688,#9689,#9690,#9691,#9692,#9693,
#9694,#9695,#9696));
#2569=EDGE_LOOP('',(#9697,#9698,#9699,#9700,#9701,#9702,#9703,#9704,#9705,
#9706,#9707,#9708));
#2570=EDGE_LOOP('',(#9709,#9710,#9711,#9712,#9713,#9714,#9715,#9716,#9717,
#9718));
#2571=EDGE_LOOP('',(#9719,#9720,#9721,#9722));
#2572=EDGE_LOOP('',(#9723,#9724,#9725,#9726));
#2573=EDGE_LOOP('',(#9727));
#2574=EDGE_LOOP('',(#9728));
#2575=EDGE_LOOP('',(#9729));
#2576=EDGE_LOOP('',(#9730));
#2577=EDGE_LOOP('',(#9731,#9732,#9733,#9734));
#2578=EDGE_LOOP('',(#9735,#9736,#9737,#9738,#9739,#9740,#9741,#9742,#9743,
#9744));
#2579=EDGE_LOOP('',(#9745,#9746,#9747,#9748));
#2580=EDGE_LOOP('',(#9749,#9750,#9751,#9752));
#2581=EDGE_LOOP('',(#9753,#9754,#9755,#9756));
#2582=EDGE_LOOP('',(#9757,#9758,#9759,#9760));
#2583=EDGE_LOOP('',(#9761,#9762,#9763,#9764));
#2584=EDGE_LOOP('',(#9765,#9766,#9767,#9768,#9769,#9770,#9771,#9772,#9773,
#9774,#9775,#9776));
#2585=EDGE_LOOP('',(#9777,#9778,#9779,#9780));
#2586=EDGE_LOOP('',(#9781,#9782,#9783,#9784));
#2587=EDGE_LOOP('',(#9785,#9786,#9787,#9788));
#2588=EDGE_LOOP('',(#9789,#9790,#9791,#9792));
#2589=EDGE_LOOP('',(#9793,#9794,#9795,#9796));
#2590=EDGE_LOOP('',(#9797,#9798,#9799,#9800));
#2591=EDGE_LOOP('',(#9801,#9802,#9803,#9804));
#2592=EDGE_LOOP('',(#9805,#9806,#9807,#9808));
#2593=EDGE_LOOP('',(#9809,#9810,#9811,#9812,#9813,#9814,#9815,#9816));
#2594=EDGE_LOOP('',(#9817,#9818,#9819,#9820,#9821,#9822,#9823,#9824));
#2595=EDGE_LOOP('',(#9825,#9826,#9827,#9828));
#2596=EDGE_LOOP('',(#9829,#9830,#9831,#9832));
#2597=EDGE_LOOP('',(#9833,#9834,#9835,#9836));
#2598=EDGE_LOOP('',(#9837,#9838,#9839,#9840));
#2599=EDGE_LOOP('',(#9841,#9842,#9843,#9844));
#2600=EDGE_LOOP('',(#9845,#9846,#9847,#9848));
#2601=EDGE_LOOP('',(#9849,#9850,#9851,#9852));
#2602=EDGE_LOOP('',(#9853,#9854,#9855,#9856));
#2603=EDGE_LOOP('',(#9857,#9858,#9859,#9860,#9861,#9862,#9863,#9864));
#2604=EDGE_LOOP('',(#9865,#9866,#9867,#9868,#9869,#9870,#9871,#9872));
#2605=EDGE_LOOP('',(#9873,#9874,#9875,#9876));
#2606=EDGE_LOOP('',(#9877,#9878,#9879,#9880));
#2607=EDGE_LOOP('',(#9881));
#2608=EDGE_LOOP('',(#9882));
#2609=EDGE_LOOP('',(#9883,#9884,#9885,#9886));
#2610=EDGE_LOOP('',(#9887));
#2611=EDGE_LOOP('',(#9888));
#2612=EDGE_LOOP('',(#9889));
#2613=EDGE_LOOP('',(#9890,#9891,#9892,#9893));
#2614=EDGE_LOOP('',(#9894,#9895,#9896,#9897));
#2615=EDGE_LOOP('',(#9898,#9899,#9900,#9901));
#2616=EDGE_LOOP('',(#9902));
#2617=EDGE_LOOP('',(#9903));
#2618=EDGE_LOOP('',(#9904,#9905,#9906,#9907));
#2619=EDGE_LOOP('',(#9908,#9909,#9910,#9911));
#2620=EDGE_LOOP('',(#9912,#9913,#9914,#9915));
#2621=EDGE_LOOP('',(#9916));
#2622=EDGE_LOOP('',(#9917,#9918,#9919,#9920));
#2623=EDGE_LOOP('',(#9921,#9922,#9923,#9924));
#2624=EDGE_LOOP('',(#9925,#9926,#9927,#9928));
#2625=EDGE_LOOP('',(#9929,#9930,#9931,#9932));
#2626=EDGE_LOOP('',(#9933,#9934,#9935,#9936));
#2627=EDGE_LOOP('',(#9937,#9938,#9939,#9940));
#2628=EDGE_LOOP('',(#9941,#9942,#9943,#9944,#9945,#9946));
#2629=EDGE_LOOP('',(#9947,#9948,#9949,#9950,#9951,#9952));
#2630=EDGE_LOOP('',(#9953,#9954,#9955,#9956));
#2631=EDGE_LOOP('',(#9957,#9958,#9959,#9960));
#2632=EDGE_LOOP('',(#9961,#9962,#9963,#9964));
#2633=EDGE_LOOP('',(#9965,#9966,#9967,#9968));
#2634=EDGE_LOOP('',(#9969,#9970,#9971,#9972));
#2635=EDGE_LOOP('',(#9973,#9974,#9975,#9976));
#2636=EDGE_LOOP('',(#9977,#9978,#9979,#9980,#9981,#9982));
#2637=EDGE_LOOP('',(#9983,#9984,#9985,#9986,#9987,#9988));
#2638=EDGE_LOOP('',(#9989));
#2639=EDGE_LOOP('',(#9990));
#2640=EDGE_LOOP('',(#9991,#9992,#9993,#9994));
#2641=EDGE_LOOP('',(#9995,#9996,#9997,#9998));
#2642=EDGE_LOOP('',(#9999,#10000,#10001,#10002));
#2643=EDGE_LOOP('',(#10003));
#2644=EDGE_LOOP('',(#10004));
#2645=EDGE_LOOP('',(#10005,#10006,#10007,#10008));
#2646=EDGE_LOOP('',(#10009,#10010,#10011,#10012));
#2647=EDGE_LOOP('',(#10013));
#2648=EDGE_LOOP('',(#10014,#10015,#10016,#10017));
#2649=EDGE_LOOP('',(#10018,#10019,#10020,#10021));
#2650=EDGE_LOOP('',(#10022,#10023,#10024,#10025));
#2651=EDGE_LOOP('',(#10026));
#2652=EDGE_LOOP('',(#10027));
#2653=EDGE_LOOP('',(#10028,#10029,#10030,#10031));
#2654=EDGE_LOOP('',(#10032,#10033,#10034,#10035));
#2655=EDGE_LOOP('',(#10036,#10037,#10038,#10039));
#2656=EDGE_LOOP('',(#10040));
#2657=EDGE_LOOP('',(#10041,#10042,#10043,#10044));
#2658=EDGE_LOOP('',(#10045,#10046,#10047,#10048));
#2659=EDGE_LOOP('',(#10049,#10050,#10051,#10052));
#2660=EDGE_LOOP('',(#10053,#10054,#10055,#10056));
#2661=EDGE_LOOP('',(#10057,#10058,#10059,#10060));
#2662=EDGE_LOOP('',(#10061,#10062,#10063,#10064));
#2663=EDGE_LOOP('',(#10065,#10066,#10067,#10068,#10069,#10070));
#2664=EDGE_LOOP('',(#10071,#10072,#10073,#10074,#10075,#10076));
#2665=LINE('',#16239,#3522);
#2666=LINE('',#16246,#3523);
#2667=LINE('',#16253,#3524);
#2668=LINE('',#16260,#3525);
#2669=LINE('',#16267,#3526);
#2670=LINE('',#16274,#3527);
#2671=LINE('',#16281,#3528);
#2672=LINE('',#16288,#3529);
#2673=LINE('',#16295,#3530);
#2674=LINE('',#16301,#3531);
#2675=LINE('',#16307,#3532);
#2676=LINE('',#16313,#3533);
#2677=LINE('',#16319,#3534);
#2678=LINE('',#16326,#3535);
#2679=LINE('',#16333,#3536);
#2680=LINE('',#16340,#3537);
#2681=LINE('',#16347,#3538);
#2682=LINE('',#16354,#3539);
#2683=LINE('',#16361,#3540);
#2684=LINE('',#16368,#3541);
#2685=LINE('',#16374,#3542);
#2686=LINE('',#16376,#3543);
#2687=LINE('',#16378,#3544);
#2688=LINE('',#16379,#3545);
#2689=LINE('',#16382,#3546);
#2690=LINE('',#16384,#3547);
#2691=LINE('',#16385,#3548);
#2692=LINE('',#16388,#3549);
#2693=LINE('',#16390,#3550);
#2694=LINE('',#16391,#3551);
#2695=LINE('',#16393,#3552);
#2696=LINE('',#16394,#3553);
#2697=LINE('',#16401,#3554);
#2698=LINE('',#16403,#3555);
#2699=LINE('',#16405,#3556);
#2700=LINE('',#16406,#3557);
#2701=LINE('',#16409,#3558);
#2702=LINE('',#16411,#3559);
#2703=LINE('',#16412,#3560);
#2704=LINE('',#16415,#3561);
#2705=LINE('',#16416,#3562);
#2706=LINE('',#16419,#3563);
#2707=LINE('',#16420,#3564);
#2708=LINE('',#16422,#3565);
#2709=LINE('',#16427,#3566);
#2710=LINE('',#16429,#3567);
#2711=LINE('',#16431,#3568);
#2712=LINE('',#16432,#3569);
#2713=LINE('',#16436,#3570);
#2714=LINE('',#16437,#3571);
#2715=LINE('',#16438,#3572);
#2716=LINE('',#16441,#3573);
#2717=LINE('',#16442,#3574);
#2718=LINE('',#16445,#3575);
#2719=LINE('',#16446,#3576);
#2720=LINE('',#16448,#3577);
#2721=LINE('',#16454,#3578);
#2722=LINE('',#16456,#3579);
#2723=LINE('',#16458,#3580);
#2724=LINE('',#16459,#3581);
#2725=LINE('',#16462,#3582);
#2726=LINE('',#16464,#3583);
#2727=LINE('',#16465,#3584);
#2728=LINE('',#16468,#3585);
#2729=LINE('',#16469,#3586);
#2730=LINE('',#16472,#3587);
#2731=LINE('',#16473,#3588);
#2732=LINE('',#16475,#3589);
#2733=LINE('',#16480,#3590);
#2734=LINE('',#16482,#3591);
#2735=LINE('',#16484,#3592);
#2736=LINE('',#16485,#3593);
#2737=LINE('',#16489,#3594);
#2738=LINE('',#16490,#3595);
#2739=LINE('',#16491,#3596);
#2740=LINE('',#16494,#3597);
#2741=LINE('',#16495,#3598);
#2742=LINE('',#16498,#3599);
#2743=LINE('',#16499,#3600);
#2744=LINE('',#16501,#3601);
#2745=LINE('',#16508,#3602);
#2746=LINE('',#16514,#3603);
#2747=LINE('',#16520,#3604);
#2748=LINE('',#16526,#3605);
#2749=LINE('',#16532,#3606);
#2750=LINE('',#16538,#3607);
#2751=LINE('',#16544,#3608);
#2752=LINE('',#16550,#3609);
#2753=LINE('',#16556,#3610);
#2754=LINE('',#16561,#3611);
#2755=LINE('',#16563,#3612);
#2756=LINE('',#16565,#3613);
#2757=LINE('',#16566,#3614);
#2758=LINE('',#16570,#3615);
#2759=LINE('',#16572,#3616);
#2760=LINE('',#16574,#3617);
#2761=LINE('',#16575,#3618);
#2762=LINE('',#16578,#3619);
#2763=LINE('',#16580,#3620);
#2764=LINE('',#16581,#3621);
#2765=LINE('',#16584,#3622);
#2766=LINE('',#16586,#3623);
#2767=LINE('',#16587,#3624);
#2768=LINE('',#16590,#3625);
#2769=LINE('',#16592,#3626);
#2770=LINE('',#16593,#3627);
#2771=LINE('',#16594,#3628);
#2772=LINE('',#16597,#3629);
#2773=LINE('',#16598,#3630);
#2774=LINE('',#16601,#3631);
#2775=LINE('',#16602,#3632);
#2776=LINE('',#16603,#3633);
#2777=LINE('',#16605,#3634);
#2778=LINE('',#16613,#3635);
#2779=LINE('',#16619,#3636);
#2780=LINE('',#16627,#3637);
#2781=LINE('',#16631,#3638);
#2782=LINE('',#16636,#3639);
#2783=LINE('',#16640,#3640);
#2784=LINE('',#16645,#3641);
#2785=LINE('',#16649,#3642);
#2786=LINE('',#16654,#3643);
#2787=LINE('',#16658,#3644);
#2788=LINE('',#16679,#3645);
#2789=LINE('',#16685,#3646);
#2790=LINE('',#16691,#3647);
#2791=LINE('',#16695,#3648);
#2792=LINE('',#16700,#3649);
#2793=LINE('',#16704,#3650);
#2794=LINE('',#16709,#3651);
#2795=LINE('',#16713,#3652);
#2796=LINE('',#16718,#3653);
#2797=LINE('',#16722,#3654);
#2798=LINE('',#16741,#3655);
#2799=LINE('',#16749,#3656);
#2800=LINE('',#16756,#3657);
#2801=LINE('',#16762,#3658);
#2802=LINE('',#16768,#3659);
#2803=LINE('',#16774,#3660);
#2804=LINE('',#16780,#3661);
#2805=LINE('',#16786,#3662);
#2806=LINE('',#16792,#3663);
#2807=LINE('',#16798,#3664);
#2808=LINE('',#16804,#3665);
#2809=LINE('',#16809,#3666);
#2810=LINE('',#16811,#3667);
#2811=LINE('',#16813,#3668);
#2812=LINE('',#16814,#3669);
#2813=LINE('',#16818,#3670);
#2814=LINE('',#16820,#3671);
#2815=LINE('',#16822,#3672);
#2816=LINE('',#16823,#3673);
#2817=LINE('',#16826,#3674);
#2818=LINE('',#16828,#3675);
#2819=LINE('',#16829,#3676);
#2820=LINE('',#16832,#3677);
#2821=LINE('',#16834,#3678);
#2822=LINE('',#16835,#3679);
#2823=LINE('',#16838,#3680);
#2824=LINE('',#16840,#3681);
#2825=LINE('',#16841,#3682);
#2826=LINE('',#16842,#3683);
#2827=LINE('',#16845,#3684);
#2828=LINE('',#16846,#3685);
#2829=LINE('',#16849,#3686);
#2830=LINE('',#16850,#3687);
#2831=LINE('',#16851,#3688);
#2832=LINE('',#16853,#3689);
#2833=LINE('',#16861,#3690);
#2834=LINE('',#16867,#3691);
#2835=LINE('',#16875,#3692);
#2836=LINE('',#16879,#3693);
#2837=LINE('',#16884,#3694);
#2838=LINE('',#16888,#3695);
#2839=LINE('',#16893,#3696);
#2840=LINE('',#16897,#3697);
#2841=LINE('',#16902,#3698);
#2842=LINE('',#16906,#3699);
#2843=LINE('',#16927,#3700);
#2844=LINE('',#16933,#3701);
#2845=LINE('',#16939,#3702);
#2846=LINE('',#16943,#3703);
#2847=LINE('',#16948,#3704);
#2848=LINE('',#16952,#3705);
#2849=LINE('',#16957,#3706);
#2850=LINE('',#16961,#3707);
#2851=LINE('',#16966,#3708);
#2852=LINE('',#16970,#3709);
#2853=LINE('',#16989,#3710);
#2854=LINE('',#16997,#3711);
#2855=LINE('',#17003,#3712);
#2856=LINE('',#17005,#3713);
#2857=LINE('',#17007,#3714);
#2858=LINE('',#17008,#3715);
#2859=LINE('',#17012,#3716);
#2860=LINE('',#17014,#3717);
#2861=LINE('',#17016,#3718);
#2862=LINE('',#17017,#3719);
#2863=LINE('',#17021,#3720);
#2864=LINE('',#17025,#3721);
#2865=LINE('',#17035,#3722);
#2866=LINE('',#17038,#3723);
#2867=LINE('',#17041,#3724);
#2868=LINE('',#17042,#3725);
#2869=LINE('',#17045,#3726);
#2870=LINE('',#17046,#3727);
#2871=LINE('',#17054,#3728);
#2872=LINE('',#17058,#3729);
#2873=LINE('',#17063,#3730);
#2874=LINE('',#17067,#3731);
#2875=LINE('',#17070,#3732);
#2876=LINE('',#17071,#3733);
#2877=LINE('',#17077,#3734);
#2878=LINE('',#17081,#3735);
#2879=LINE('',#17086,#3736);
#2880=LINE('',#17090,#3737);
#2881=LINE('',#17093,#3738);
#2882=LINE('',#17094,#3739);
#2883=LINE('',#17099,#3740);
#2884=LINE('',#17101,#3741);
#2885=LINE('',#17103,#3742);
#2886=LINE('',#17105,#3743);
#2887=LINE('',#17107,#3744);
#2888=LINE('',#17109,#3745);
#2889=LINE('',#17111,#3746);
#2890=LINE('',#17113,#3747);
#2891=LINE('',#17114,#3748);
#2892=LINE('',#17115,#3749);
#2893=LINE('',#17118,#3750);
#2894=LINE('',#17119,#3751);
#2895=LINE('',#17122,#3752);
#2896=LINE('',#17123,#3753);
#2897=LINE('',#17125,#3754);
#2898=LINE('',#17129,#3755);
#2899=LINE('',#17133,#3756);
#2900=LINE('',#17136,#3757);
#2901=LINE('',#17138,#3758);
#2902=LINE('',#17139,#3759);
#2903=LINE('',#17142,#3760);
#2904=LINE('',#17144,#3761);
#2905=LINE('',#17145,#3762);
#2906=LINE('',#17147,#3763);
#2907=LINE('',#17150,#3764);
#2908=LINE('',#17151,#3765);
#2909=LINE('',#17153,#3766);
#2910=LINE('',#17154,#3767);
#2911=LINE('',#17156,#3768);
#2912=LINE('',#17158,#3769);
#2913=LINE('',#17165,#3770);
#2914=LINE('',#17169,#3771);
#2915=LINE('',#17174,#3772);
#2916=LINE('',#17178,#3773);
#2917=LINE('',#17181,#3774);
#2918=LINE('',#17182,#3775);
#2919=LINE('',#17188,#3776);
#2920=LINE('',#17192,#3777);
#2921=LINE('',#17197,#3778);
#2922=LINE('',#17201,#3779);
#2923=LINE('',#17204,#3780);
#2924=LINE('',#17205,#3781);
#2925=LINE('',#17210,#3782);
#2926=LINE('',#17212,#3783);
#2927=LINE('',#17214,#3784);
#2928=LINE('',#17216,#3785);
#2929=LINE('',#17218,#3786);
#2930=LINE('',#17220,#3787);
#2931=LINE('',#17222,#3788);
#2932=LINE('',#17224,#3789);
#2933=LINE('',#17225,#3790);
#2934=LINE('',#17226,#3791);
#2935=LINE('',#17229,#3792);
#2936=LINE('',#17230,#3793);
#2937=LINE('',#17233,#3794);
#2938=LINE('',#17234,#3795);
#2939=LINE('',#17236,#3796);
#2940=LINE('',#17240,#3797);
#2941=LINE('',#17244,#3798);
#2942=LINE('',#17247,#3799);
#2943=LINE('',#17249,#3800);
#2944=LINE('',#17250,#3801);
#2945=LINE('',#17253,#3802);
#2946=LINE('',#17255,#3803);
#2947=LINE('',#17256,#3804);
#2948=LINE('',#17258,#3805);
#2949=LINE('',#17261,#3806);
#2950=LINE('',#17262,#3807);
#2951=LINE('',#17264,#3808);
#2952=LINE('',#17265,#3809);
#2953=LINE('',#17267,#3810);
#2954=LINE('',#17269,#3811);
#2955=LINE('',#17286,#3812);
#2956=LINE('',#17292,#3813);
#2957=LINE('',#17296,#3814);
#2958=LINE('',#17302,#3815);
#2959=LINE('',#17307,#3816);
#2960=LINE('',#17322,#3817);
#2961=LINE('',#17331,#3818);
#2962=LINE('',#17335,#3819);
#2963=LINE('',#17339,#3820);
#2964=LINE('',#17342,#3821);
#2965=LINE('',#17495,#3822);
#2966=LINE('',#17791,#3823);
#2967=LINE('',#17833,#3824);
#2968=LINE('',#17838,#3825);
#2969=LINE('',#17847,#3826);
#2970=LINE('',#17852,#3827);
#2971=LINE('',#17862,#3828);
#2972=LINE('',#17864,#3829);
#2973=LINE('',#17866,#3830);
#2974=LINE('',#17867,#3831);
#2975=LINE('',#17870,#3832);
#2976=LINE('',#17872,#3833);
#2977=LINE('',#17873,#3834);
#2978=LINE('',#17876,#3835);
#2979=LINE('',#17878,#3836);
#2980=LINE('',#17879,#3837);
#2981=LINE('',#17882,#3838);
#2982=LINE('',#17884,#3839);
#2983=LINE('',#17885,#3840);
#2984=LINE('',#17888,#3841);
#2985=LINE('',#17890,#3842);
#2986=LINE('',#17891,#3843);
#2987=LINE('',#17894,#3844);
#2988=LINE('',#17896,#3845);
#2989=LINE('',#17897,#3846);
#2990=LINE('',#17900,#3847);
#2991=LINE('',#17902,#3848);
#2992=LINE('',#17903,#3849);
#2993=LINE('',#17906,#3850);
#2994=LINE('',#17908,#3851);
#2995=LINE('',#17909,#3852);
#2996=LINE('',#17912,#3853);
#2997=LINE('',#17914,#3854);
#2998=LINE('',#17915,#3855);
#2999=LINE('',#17919,#3856);
#3000=LINE('',#17921,#3857);
#3001=LINE('',#17923,#3858);
#3002=LINE('',#17924,#3859);
#3003=LINE('',#17927,#3860);
#3004=LINE('',#17929,#3861);
#3005=LINE('',#17930,#3862);
#3006=LINE('',#17933,#3863);
#3007=LINE('',#17935,#3864);
#3008=LINE('',#17936,#3865);
#3009=LINE('',#17939,#3866);
#3010=LINE('',#17941,#3867);
#3011=LINE('',#17942,#3868);
#3012=LINE('',#17945,#3869);
#3013=LINE('',#17947,#3870);
#3014=LINE('',#17948,#3871);
#3015=LINE('',#17951,#3872);
#3016=LINE('',#17953,#3873);
#3017=LINE('',#17954,#3874);
#3018=LINE('',#17957,#3875);
#3019=LINE('',#17959,#3876);
#3020=LINE('',#17960,#3877);
#3021=LINE('',#17963,#3878);
#3022=LINE('',#17965,#3879);
#3023=LINE('',#17966,#3880);
#3024=LINE('',#17969,#3881);
#3025=LINE('',#17971,#3882);
#3026=LINE('',#17972,#3883);
#3027=LINE('',#17976,#3884);
#3028=LINE('',#17978,#3885);
#3029=LINE('',#17980,#3886);
#3030=LINE('',#17981,#3887);
#3031=LINE('',#17984,#3888);
#3032=LINE('',#17986,#3889);
#3033=LINE('',#17987,#3890);
#3034=LINE('',#17990,#3891);
#3035=LINE('',#17992,#3892);
#3036=LINE('',#17993,#3893);
#3037=LINE('',#17996,#3894);
#3038=LINE('',#17998,#3895);
#3039=LINE('',#17999,#3896);
#3040=LINE('',#18002,#3897);
#3041=LINE('',#18004,#3898);
#3042=LINE('',#18005,#3899);
#3043=LINE('',#18008,#3900);
#3044=LINE('',#18010,#3901);
#3045=LINE('',#18011,#3902);
#3046=LINE('',#18014,#3903);
#3047=LINE('',#18016,#3904);
#3048=LINE('',#18017,#3905);
#3049=LINE('',#18020,#3906);
#3050=LINE('',#18022,#3907);
#3051=LINE('',#18023,#3908);
#3052=LINE('',#18026,#3909);
#3053=LINE('',#18028,#3910);
#3054=LINE('',#18029,#3911);
#3055=LINE('',#18033,#3912);
#3056=LINE('',#18035,#3913);
#3057=LINE('',#18037,#3914);
#3058=LINE('',#18038,#3915);
#3059=LINE('',#18041,#3916);
#3060=LINE('',#18043,#3917);
#3061=LINE('',#18044,#3918);
#3062=LINE('',#18047,#3919);
#3063=LINE('',#18049,#3920);
#3064=LINE('',#18050,#3921);
#3065=LINE('',#18053,#3922);
#3066=LINE('',#18055,#3923);
#3067=LINE('',#18056,#3924);
#3068=LINE('',#18059,#3925);
#3069=LINE('',#18061,#3926);
#3070=LINE('',#18062,#3927);
#3071=LINE('',#18065,#3928);
#3072=LINE('',#18067,#3929);
#3073=LINE('',#18068,#3930);
#3074=LINE('',#18071,#3931);
#3075=LINE('',#18073,#3932);
#3076=LINE('',#18074,#3933);
#3077=LINE('',#18077,#3934);
#3078=LINE('',#18079,#3935);
#3079=LINE('',#18080,#3936);
#3080=LINE('',#18083,#3937);
#3081=LINE('',#18085,#3938);
#3082=LINE('',#18086,#3939);
#3083=LINE('',#18091,#3940);
#3084=LINE('',#18095,#3941);
#3085=LINE('',#18097,#3942);
#3086=LINE('',#18098,#3943);
#3087=LINE('',#18101,#3944);
#3088=LINE('',#18103,#3945);
#3089=LINE('',#18104,#3946);
#3090=LINE('',#18106,#3947);
#3091=LINE('',#18107,#3948);
#3092=LINE('',#18110,#3949);
#3093=LINE('',#18112,#3950);
#3094=LINE('',#18113,#3951);
#3095=LINE('',#18115,#3952);
#3096=LINE('',#18116,#3953);
#3097=LINE('',#18119,#3954);
#3098=LINE('',#18121,#3955);
#3099=LINE('',#18122,#3956);
#3100=LINE('',#18124,#3957);
#3101=LINE('',#18125,#3958);
#3102=LINE('',#18127,#3959);
#3103=LINE('',#18128,#3960);
#3104=LINE('',#18135,#3961);
#3105=LINE('',#18137,#3962);
#3106=LINE('',#18139,#3963);
#3107=LINE('',#18140,#3964);
#3108=LINE('',#18143,#3965);
#3109=LINE('',#18145,#3966);
#3110=LINE('',#18146,#3967);
#3111=LINE('',#18149,#3968);
#3112=LINE('',#18151,#3969);
#3113=LINE('',#18152,#3970);
#3114=LINE('',#18157,#3971);
#3115=LINE('',#18159,#3972);
#3116=LINE('',#18161,#3973);
#3117=LINE('',#18163,#3974);
#3118=LINE('',#18165,#3975);
#3119=LINE('',#18167,#3976);
#3120=LINE('',#18168,#3977);
#3121=LINE('',#18171,#3978);
#3122=LINE('',#18172,#3979);
#3123=LINE('',#18175,#3980);
#3124=LINE('',#18176,#3981);
#3125=LINE('',#18179,#3982);
#3126=LINE('',#18181,#3983);
#3127=LINE('',#18183,#3984);
#3128=LINE('',#18185,#3985);
#3129=LINE('',#18186,#3986);
#3130=LINE('',#18188,#3987);
#3131=LINE('',#18191,#3988);
#3132=LINE('',#18194,#3989);
#3133=LINE('',#18198,#3990);
#3134=LINE('',#18205,#3991);
#3135=LINE('',#18207,#3992);
#3136=LINE('',#18209,#3993);
#3137=LINE('',#18215,#3994);
#3138=LINE('',#18217,#3995);
#3139=LINE('',#18219,#3996);
#3140=LINE('',#18220,#3997);
#3141=LINE('',#18223,#3998);
#3142=LINE('',#18225,#3999);
#3143=LINE('',#18226,#4000);
#3144=LINE('',#18229,#4001);
#3145=LINE('',#18231,#4002);
#3146=LINE('',#18232,#4003);
#3147=LINE('',#18235,#4004);
#3148=LINE('',#18237,#4005);
#3149=LINE('',#18238,#4006);
#3150=LINE('',#18241,#4007);
#3151=LINE('',#18243,#4008);
#3152=LINE('',#18244,#4009);
#3153=LINE('',#18246,#4010);
#3154=LINE('',#18247,#4011);
#3155=LINE('',#18259,#4012);
#3156=LINE('',#18263,#4013);
#3157=LINE('',#18267,#4014);
#3158=LINE('',#18274,#4015);
#3159=LINE('',#18276,#4016);
#3160=LINE('',#18282,#4017);
#3161=LINE('',#18291,#4018);
#3162=LINE('',#18300,#4019);
#3163=LINE('',#18309,#4020);
#3164=LINE('',#18317,#4021);
#3165=LINE('',#18321,#4022);
#3166=LINE('',#18325,#4023);
#3167=LINE('',#18329,#4024);
#3168=LINE('',#18333,#4025);
#3169=LINE('',#18335,#4026);
#3170=LINE('',#18337,#4027);
#3171=LINE('',#18338,#4028);
#3172=LINE('',#18341,#4029);
#3173=LINE('',#18343,#4030);
#3174=LINE('',#18344,#4031);
#3175=LINE('',#18347,#4032);
#3176=LINE('',#18349,#4033);
#3177=LINE('',#18350,#4034);
#3178=LINE('',#18353,#4035);
#3179=LINE('',#18355,#4036);
#3180=LINE('',#18356,#4037);
#3181=LINE('',#18359,#4038);
#3182=LINE('',#18361,#4039);
#3183=LINE('',#18362,#4040);
#3184=LINE('',#18365,#4041);
#3185=LINE('',#18367,#4042);
#3186=LINE('',#18368,#4043);
#3187=LINE('',#18371,#4044);
#3188=LINE('',#18373,#4045);
#3189=LINE('',#18374,#4046);
#3190=LINE('',#18377,#4047);
#3191=LINE('',#18379,#4048);
#3192=LINE('',#18380,#4049);
#3193=LINE('',#18383,#4050);
#3194=LINE('',#18385,#4051);
#3195=LINE('',#18386,#4052);
#3196=LINE('',#18389,#4053);
#3197=LINE('',#18391,#4054);
#3198=LINE('',#18392,#4055);
#3199=LINE('',#18395,#4056);
#3200=LINE('',#18397,#4057);
#3201=LINE('',#18398,#4058);
#3202=LINE('',#18400,#4059);
#3203=LINE('',#18401,#4060);
#3204=LINE('',#18410,#4061);
#3205=LINE('',#18424,#4062);
#3206=LINE('',#18427,#4063);
#3207=LINE('',#18433,#4064);
#3208=LINE('',#18439,#4065);
#3209=LINE('',#18447,#4066);
#3210=LINE('',#18454,#4067);
#3211=LINE('',#18460,#4068);
#3212=LINE('',#18469,#4069);
#3213=LINE('',#18475,#4070);
#3214=LINE('',#18484,#4071);
#3215=LINE('',#18493,#4072);
#3216=LINE('',#18502,#4073);
#3217=LINE('',#18508,#4074);
#3218=LINE('',#18518,#4075);
#3219=LINE('',#18532,#4076);
#3220=LINE('',#18535,#4077);
#3221=LINE('',#18541,#4078);
#3222=LINE('',#18547,#4079);
#3223=LINE('',#18555,#4080);
#3224=LINE('',#18562,#4081);
#3225=LINE('',#18568,#4082);
#3226=LINE('',#18577,#4083);
#3227=LINE('',#18583,#4084);
#3228=LINE('',#18592,#4085);
#3229=LINE('',#18601,#4086);
#3230=LINE('',#18610,#4087);
#3231=LINE('',#18616,#4088);
#3232=LINE('',#18664,#4089);
#3233=LINE('',#18748,#4090);
#3234=LINE('',#18792,#4091);
#3235=LINE('',#18794,#4092);
#3236=LINE('',#18880,#4093);
#3237=LINE('',#18957,#4094);
#3238=LINE('',#18961,#4095);
#3239=LINE('',#18963,#4096);
#3240=LINE('',#19052,#4097);
#3241=LINE('',#19140,#4098);
#3242=LINE('',#19143,#4099);
#3243=LINE('',#19144,#4100);
#3244=LINE('',#19146,#4101);
#3245=LINE('',#19148,#4102);
#3246=LINE('',#19150,#4103);
#3247=LINE('',#19152,#4104);
#3248=LINE('',#19154,#4105);
#3249=LINE('',#19156,#4106);
#3250=LINE('',#19158,#4107);
#3251=LINE('',#19160,#4108);
#3252=LINE('',#19162,#4109);
#3253=LINE('',#19164,#4110);
#3254=LINE('',#19166,#4111);
#3255=LINE('',#19168,#4112);
#3256=LINE('',#19170,#4113);
#3257=LINE('',#19172,#4114);
#3258=LINE('',#19174,#4115);
#3259=LINE('',#19176,#4116);
#3260=LINE('',#19178,#4117);
#3261=LINE('',#19180,#4118);
#3262=LINE('',#19182,#4119);
#3263=LINE('',#19184,#4120);
#3264=LINE('',#19186,#4121);
#3265=LINE('',#19188,#4122);
#3266=LINE('',#19190,#4123);
#3267=LINE('',#19192,#4124);
#3268=LINE('',#19194,#4125);
#3269=LINE('',#19196,#4126);
#3270=LINE('',#19198,#4127);
#3271=LINE('',#19200,#4128);
#3272=LINE('',#19202,#4129);
#3273=LINE('',#19204,#4130);
#3274=LINE('',#19206,#4131);
#3275=LINE('',#19208,#4132);
#3276=LINE('',#19210,#4133);
#3277=LINE('',#19212,#4134);
#3278=LINE('',#19214,#4135);
#3279=LINE('',#19216,#4136);
#3280=LINE('',#19218,#4137);
#3281=LINE('',#19220,#4138);
#3282=LINE('',#19228,#4139);
#3283=LINE('',#19237,#4140);
#3284=LINE('',#19244,#4141);
#3285=LINE('',#19248,#4142);
#3286=LINE('',#19254,#4143);
#3287=LINE('',#19260,#4144);
#3288=LINE('',#19266,#4145);
#3289=LINE('',#19272,#4146);
#3290=LINE('',#19277,#4147);
#3291=LINE('',#19279,#4148);
#3292=LINE('',#19281,#4149);
#3293=LINE('',#19282,#4150);
#3294=LINE('',#19285,#4151);
#3295=LINE('',#19287,#4152);
#3296=LINE('',#19288,#4153);
#3297=LINE('',#19291,#4154);
#3298=LINE('',#19293,#4155);
#3299=LINE('',#19294,#4156);
#3300=LINE('',#19296,#4157);
#3301=LINE('',#19297,#4158);
#3302=LINE('',#19305,#4159);
#3303=LINE('',#19312,#4160);
#3304=LINE('',#19318,#4161);
#3305=LINE('',#19322,#4162);
#3306=LINE('',#19323,#4163);
#3307=LINE('',#19326,#4164);
#3308=LINE('',#19329,#4165);
#3309=LINE('',#19333,#4166);
#3310=LINE('',#19337,#4167);
#3311=LINE('',#19341,#4168);
#3312=LINE('',#19343,#4169);
#3313=LINE('',#19344,#4170);
#3314=LINE('',#19347,#4171);
#3315=LINE('',#19349,#4172);
#3316=LINE('',#19351,#4173);
#3317=LINE('',#19353,#4174);
#3318=LINE('',#19354,#4175);
#3319=LINE('',#19356,#4176);
#3320=LINE('',#19358,#4177);
#3321=LINE('',#19359,#4178);
#3322=LINE('',#19364,#4179);
#3323=LINE('',#19371,#4180);
#3324=LINE('',#19376,#4181);
#3325=LINE('',#19378,#4182);
#3326=LINE('',#19379,#4183);
#3327=LINE('',#19382,#4184);
#3328=LINE('',#19383,#4185);
#3329=LINE('',#19385,#4186);
#3330=LINE('',#19387,#4187);
#3331=LINE('',#19388,#4188);
#3332=LINE('',#19395,#4189);
#3333=LINE('',#19397,#4190);
#3334=LINE('',#19399,#4191);
#3335=LINE('',#19400,#4192);
#3336=LINE('',#19403,#4193);
#3337=LINE('',#19405,#4194);
#3338=LINE('',#19406,#4195);
#3339=LINE('',#19409,#4196);
#3340=LINE('',#19411,#4197);
#3341=LINE('',#19412,#4198);
#3342=LINE('',#19414,#4199);
#3343=LINE('',#19415,#4200);
#3344=LINE('',#19423,#4201);
#3345=LINE('',#19427,#4202);
#3346=LINE('',#19431,#4203);
#3347=LINE('',#19435,#4204);
#3348=LINE('',#19439,#4205);
#3349=LINE('',#19443,#4206);
#3350=LINE('',#19447,#4207);
#3351=LINE('',#19451,#4208);
#3352=LINE('',#19455,#4209);
#3353=LINE('',#19459,#4210);
#3354=LINE('',#19463,#4211);
#3355=LINE('',#19467,#4212);
#3356=LINE('',#19471,#4213);
#3357=LINE('',#19475,#4214);
#3358=LINE('',#19479,#4215);
#3359=LINE('',#19483,#4216);
#3360=LINE('',#19485,#4217);
#3361=LINE('',#19487,#4218);
#3362=LINE('',#19489,#4219);
#3363=LINE('',#19491,#4220);
#3364=LINE('',#19493,#4221);
#3365=LINE('',#19494,#4222);
#3366=LINE('',#19496,#4223);
#3367=LINE('',#19498,#4224);
#3368=LINE('',#19500,#4225);
#3369=LINE('',#19502,#4226);
#3370=LINE('',#19504,#4227);
#3371=LINE('',#19505,#4228);
#3372=LINE('',#19508,#4229);
#3373=LINE('',#19510,#4230);
#3374=LINE('',#19512,#4231);
#3375=LINE('',#19514,#4232);
#3376=LINE('',#19515,#4233);
#3377=LINE('',#19517,#4234);
#3378=LINE('',#19519,#4235);
#3379=LINE('',#19521,#4236);
#3380=LINE('',#19523,#4237);
#3381=LINE('',#19524,#4238);
#3382=LINE('',#19527,#4239);
#3383=LINE('',#19528,#4240);
#3384=LINE('',#19531,#4241);
#3385=LINE('',#19532,#4242);
#3386=LINE('',#19535,#4243);
#3387=LINE('',#19536,#4244);
#3388=LINE('',#19539,#4245);
#3389=LINE('',#19540,#4246);
#3390=LINE('',#19542,#4247);
#3391=LINE('',#19545,#4248);
#3392=LINE('',#19546,#4249);
#3393=LINE('',#19549,#4250);
#3394=LINE('',#19550,#4251);
#3395=LINE('',#19553,#4252);
#3396=LINE('',#19554,#4253);
#3397=LINE('',#19557,#4254);
#3398=LINE('',#19558,#4255);
#3399=LINE('',#19560,#4256);
#3400=LINE('',#19566,#4257);
#3401=LINE('',#19568,#4258);
#3402=LINE('',#19570,#4259);
#3403=LINE('',#19571,#4260);
#3404=LINE('',#19574,#4261);
#3405=LINE('',#19576,#4262);
#3406=LINE('',#19577,#4263);
#3407=LINE('',#19580,#4264);
#3408=LINE('',#19582,#4265);
#3409=LINE('',#19583,#4266);
#3410=LINE('',#19586,#4267);
#3411=LINE('',#19588,#4268);
#3412=LINE('',#19589,#4269);
#3413=LINE('',#19592,#4270);
#3414=LINE('',#19594,#4271);
#3415=LINE('',#19595,#4272);
#3416=LINE('',#19598,#4273);
#3417=LINE('',#19600,#4274);
#3418=LINE('',#19601,#4275);
#3419=LINE('',#19604,#4276);
#3420=LINE('',#19606,#4277);
#3421=LINE('',#19607,#4278);
#3422=LINE('',#19609,#4279);
#3423=LINE('',#19610,#4280);
#3424=LINE('',#19617,#4281);
#3425=LINE('',#19619,#4282);
#3426=LINE('',#19621,#4283);
#3427=LINE('',#19622,#4284);
#3428=LINE('',#19625,#4285);
#3429=LINE('',#19627,#4286);
#3430=LINE('',#19628,#4287);
#3431=LINE('',#19631,#4288);
#3432=LINE('',#19633,#4289);
#3433=LINE('',#19634,#4290);
#3434=LINE('',#19637,#4291);
#3435=LINE('',#19639,#4292);
#3436=LINE('',#19640,#4293);
#3437=LINE('',#19643,#4294);
#3438=LINE('',#19645,#4295);
#3439=LINE('',#19646,#4296);
#3440=LINE('',#19649,#4297);
#3441=LINE('',#19651,#4298);
#3442=LINE('',#19652,#4299);
#3443=LINE('',#19655,#4300);
#3444=LINE('',#19657,#4301);
#3445=LINE('',#19658,#4302);
#3446=LINE('',#19660,#4303);
#3447=LINE('',#19661,#4304);
#3448=LINE('',#19672,#4305);
#3449=LINE('',#19676,#4306);
#3450=LINE('',#19683,#4307);
#3451=LINE('',#19693,#4308);
#3452=LINE('',#19697,#4309);
#3453=LINE('',#19701,#4310);
#3454=LINE('',#19708,#4311);
#3455=LINE('',#19712,#4312);
#3456=LINE('',#19716,#4313);
#3457=LINE('',#19721,#4314);
#3458=LINE('',#19723,#4315);
#3459=LINE('',#19725,#4316);
#3460=LINE('',#19726,#4317);
#3461=LINE('',#19729,#4318);
#3462=LINE('',#19731,#4319);
#3463=LINE('',#19732,#4320);
#3464=LINE('',#19735,#4321);
#3465=LINE('',#19737,#4322);
#3466=LINE('',#19738,#4323);
#3467=LINE('',#19741,#4324);
#3468=LINE('',#19743,#4325);
#3469=LINE('',#19744,#4326);
#3470=LINE('',#19747,#4327);
#3471=LINE('',#19749,#4328);
#3472=LINE('',#19750,#4329);
#3473=LINE('',#19752,#4330);
#3474=LINE('',#19753,#4331);
#3475=LINE('',#19760,#4332);
#3476=LINE('',#19762,#4333);
#3477=LINE('',#19764,#4334);
#3478=LINE('',#19765,#4335);
#3479=LINE('',#19768,#4336);
#3480=LINE('',#19770,#4337);
#3481=LINE('',#19771,#4338);
#3482=LINE('',#19774,#4339);
#3483=LINE('',#19776,#4340);
#3484=LINE('',#19777,#4341);
#3485=LINE('',#19780,#4342);
#3486=LINE('',#19782,#4343);
#3487=LINE('',#19783,#4344);
#3488=LINE('',#19786,#4345);
#3489=LINE('',#19788,#4346);
#3490=LINE('',#19789,#4347);
#3491=LINE('',#19791,#4348);
#3492=LINE('',#19792,#4349);
#3493=LINE('',#19804,#4350);
#3494=LINE('',#19808,#4351);
#3495=LINE('',#19812,#4352);
#3496=LINE('',#19819,#4353);
#3497=LINE('',#19821,#4354);
#3498=LINE('',#19829,#4355);
#3499=LINE('',#19833,#4356);
#3500=LINE('',#19837,#4357);
#3501=LINE('',#19844,#4358);
#3502=LINE('',#19848,#4359);
#3503=LINE('',#19852,#4360);
#3504=LINE('',#19857,#4361);
#3505=LINE('',#19859,#4362);
#3506=LINE('',#19861,#4363);
#3507=LINE('',#19862,#4364);
#3508=LINE('',#19865,#4365);
#3509=LINE('',#19867,#4366);
#3510=LINE('',#19868,#4367);
#3511=LINE('',#19871,#4368);
#3512=LINE('',#19873,#4369);
#3513=LINE('',#19874,#4370);
#3514=LINE('',#19877,#4371);
#3515=LINE('',#19879,#4372);
#3516=LINE('',#19880,#4373);
#3517=LINE('',#19883,#4374);
#3518=LINE('',#19885,#4375);
#3519=LINE('',#19886,#4376);
#3520=LINE('',#19888,#4377);
#3521=LINE('',#19889,#4378);
#3522=VECTOR('',#12795,0.164999999999999);
#3523=VECTOR('',#12804,0.164999999999999);
#3524=VECTOR('',#12813,0.165);
#3525=VECTOR('',#12822,0.165);
#3526=VECTOR('',#12831,0.164999999999999);
#3527=VECTOR('',#12840,0.164999999999999);
#3528=VECTOR('',#12849,0.164999999999999);
#3529=VECTOR('',#12858,0.165);
#3530=VECTOR('',#12867,0.274999999999999);
#3531=VECTOR('',#12874,0.275);
#3532=VECTOR('',#12881,0.274999999999999);
#3533=VECTOR('',#12888,0.275);
#3534=VECTOR('',#12895,0.164999999999999);
#3535=VECTOR('',#12904,0.164999999999999);
#3536=VECTOR('',#12913,0.164999999999999);
#3537=VECTOR('',#12922,0.164999999999999);
#3538=VECTOR('',#12931,0.165);
#3539=VECTOR('',#12940,0.165);
#3540=VECTOR('',#12949,0.165);
#3541=VECTOR('',#12958,0.165);
#3542=VECTOR('',#12965,1.);
#3543=VECTOR('',#12966,1.);
#3544=VECTOR('',#12967,1.);
#3545=VECTOR('',#12968,1.);
#3546=VECTOR('',#12971,1.);
#3547=VECTOR('',#12972,1.);
#3548=VECTOR('',#12973,1.);
#3549=VECTOR('',#12976,1.);
#3550=VECTOR('',#12977,1.);
#3551=VECTOR('',#12978,1.);
#3552=VECTOR('',#12981,1.);
#3553=VECTOR('',#12982,1.);
#3554=VECTOR('',#12991,1.);
#3555=VECTOR('',#12992,1.);
#3556=VECTOR('',#12993,1.);
#3557=VECTOR('',#12994,1.);
#3558=VECTOR('',#12997,1.);
#3559=VECTOR('',#12998,1.);
#3560=VECTOR('',#12999,1.);
#3561=VECTOR('',#13002,1.);
#3562=VECTOR('',#13003,1.);
#3563=VECTOR('',#13006,1.);
#3564=VECTOR('',#13007,1.);
#3565=VECTOR('',#13010,1.);
#3566=VECTOR('',#13015,1.);
#3567=VECTOR('',#13016,1.);
#3568=VECTOR('',#13017,1.);
#3569=VECTOR('',#13018,1.);
#3570=VECTOR('',#13021,1.);
#3571=VECTOR('',#13022,1.);
#3572=VECTOR('',#13023,1.);
#3573=VECTOR('',#13026,1.);
#3574=VECTOR('',#13027,1.);
#3575=VECTOR('',#13030,1.);
#3576=VECTOR('',#13031,1.);
#3577=VECTOR('',#13034,1.);
#3578=VECTOR('',#13041,1.);
#3579=VECTOR('',#13042,1.);
#3580=VECTOR('',#13043,1.);
#3581=VECTOR('',#13044,1.);
#3582=VECTOR('',#13047,1.);
#3583=VECTOR('',#13048,1.);
#3584=VECTOR('',#13049,1.);
#3585=VECTOR('',#13052,1.);
#3586=VECTOR('',#13053,1.);
#3587=VECTOR('',#13056,1.);
#3588=VECTOR('',#13057,1.);
#3589=VECTOR('',#13060,1.);
#3590=VECTOR('',#13065,1.);
#3591=VECTOR('',#13066,1.);
#3592=VECTOR('',#13067,1.);
#3593=VECTOR('',#13068,1.);
#3594=VECTOR('',#13071,1.);
#3595=VECTOR('',#13072,1.);
#3596=VECTOR('',#13073,1.);
#3597=VECTOR('',#13076,1.);
#3598=VECTOR('',#13077,1.);
#3599=VECTOR('',#13080,1.);
#3600=VECTOR('',#13081,1.);
#3601=VECTOR('',#13084,1.);
#3602=VECTOR('',#13093,0.165);
#3603=VECTOR('',#13100,0.165);
#3604=VECTOR('',#13107,0.165);
#3605=VECTOR('',#13114,0.165);
#3606=VECTOR('',#13121,1.5);
#3607=VECTOR('',#13128,0.225);
#3608=VECTOR('',#13135,0.225);
#3609=VECTOR('',#13142,0.225);
#3610=VECTOR('',#13149,0.225);
#3611=VECTOR('',#13154,1.);
#3612=VECTOR('',#13155,1.);
#3613=VECTOR('',#13156,1.);
#3614=VECTOR('',#13157,1.);
#3615=VECTOR('',#13160,1.);
#3616=VECTOR('',#13161,1.);
#3617=VECTOR('',#13162,1.);
#3618=VECTOR('',#13163,1.);
#3619=VECTOR('',#13166,1.);
#3620=VECTOR('',#13167,1.);
#3621=VECTOR('',#13168,1.);
#3622=VECTOR('',#13171,1.);
#3623=VECTOR('',#13172,1.);
#3624=VECTOR('',#13173,1.);
#3625=VECTOR('',#13176,1.);
#3626=VECTOR('',#13177,1.);
#3627=VECTOR('',#13178,1.);
#3628=VECTOR('',#13179,1.);
#3629=VECTOR('',#13182,1.);
#3630=VECTOR('',#13183,1.);
#3631=VECTOR('',#13186,1.);
#3632=VECTOR('',#13187,1.);
#3633=VECTOR('',#13188,1.);
#3634=VECTOR('',#13191,1.);
#3635=VECTOR('',#13202,1.1);
#3636=VECTOR('',#13209,1.49);
#3637=VECTOR('',#13220,1.);
#3638=VECTOR('',#13223,1.);
#3639=VECTOR('',#13228,1.);
#3640=VECTOR('',#13231,1.);
#3641=VECTOR('',#13236,1.);
#3642=VECTOR('',#13239,1.);
#3643=VECTOR('',#13244,1.);
#3644=VECTOR('',#13247,1.);
#3645=VECTOR('',#13282,1.49);
#3646=VECTOR('',#13291,1.1);
#3647=VECTOR('',#13298,1.);
#3648=VECTOR('',#13301,1.);
#3649=VECTOR('',#13306,1.);
#3650=VECTOR('',#13309,1.);
#3651=VECTOR('',#13314,1.);
#3652=VECTOR('',#13317,1.);
#3653=VECTOR('',#13322,1.);
#3654=VECTOR('',#13325,1.);
#3655=VECTOR('',#13358,1.49);
#3656=VECTOR('',#13369,1.1);
#3657=VECTOR('',#13378,0.164999999999999);
#3658=VECTOR('',#13385,0.164999999999999);
#3659=VECTOR('',#13392,0.164999999999999);
#3660=VECTOR('',#13399,0.164999999999999);
#3661=VECTOR('',#13406,1.5);
#3662=VECTOR('',#13413,0.225000000000001);
#3663=VECTOR('',#13420,0.225000000000001);
#3664=VECTOR('',#13427,0.225000000000001);
#3665=VECTOR('',#13434,0.225000000000001);
#3666=VECTOR('',#13439,1.);
#3667=VECTOR('',#13440,1.);
#3668=VECTOR('',#13441,1.);
#3669=VECTOR('',#13442,1.);
#3670=VECTOR('',#13445,1.);
#3671=VECTOR('',#13446,1.);
#3672=VECTOR('',#13447,1.);
#3673=VECTOR('',#13448,1.);
#3674=VECTOR('',#13451,1.);
#3675=VECTOR('',#13452,1.);
#3676=VECTOR('',#13453,1.);
#3677=VECTOR('',#13456,1.);
#3678=VECTOR('',#13457,1.);
#3679=VECTOR('',#13458,1.);
#3680=VECTOR('',#13461,1.);
#3681=VECTOR('',#13462,1.);
#3682=VECTOR('',#13463,1.);
#3683=VECTOR('',#13464,1.);
#3684=VECTOR('',#13467,1.);
#3685=VECTOR('',#13468,1.);
#3686=VECTOR('',#13471,1.);
#3687=VECTOR('',#13472,1.);
#3688=VECTOR('',#13473,1.);
#3689=VECTOR('',#13476,1.);
#3690=VECTOR('',#13487,1.1);
#3691=VECTOR('',#13494,1.49);
#3692=VECTOR('',#13505,1.);
#3693=VECTOR('',#13508,1.);
#3694=VECTOR('',#13513,1.);
#3695=VECTOR('',#13516,1.);
#3696=VECTOR('',#13521,1.);
#3697=VECTOR('',#13524,1.);
#3698=VECTOR('',#13529,1.);
#3699=VECTOR('',#13532,1.);
#3700=VECTOR('',#13567,1.49);
#3701=VECTOR('',#13576,1.1);
#3702=VECTOR('',#13583,1.);
#3703=VECTOR('',#13586,1.);
#3704=VECTOR('',#13591,1.);
#3705=VECTOR('',#13594,1.);
#3706=VECTOR('',#13599,1.);
#3707=VECTOR('',#13602,1.);
#3708=VECTOR('',#13607,1.);
#3709=VECTOR('',#13610,1.);
#3710=VECTOR('',#13643,1.49);
#3711=VECTOR('',#13654,1.1);
#3712=VECTOR('',#13661,1.);
#3713=VECTOR('',#13662,1.);
#3714=VECTOR('',#13663,1.);
#3715=VECTOR('',#13664,1.);
#3716=VECTOR('',#13667,1.);
#3717=VECTOR('',#13668,1.);
#3718=VECTOR('',#13669,1.);
#3719=VECTOR('',#13670,1.);
#3720=VECTOR('',#13673,1.);
#3721=VECTOR('',#13676,1.);
#3722=VECTOR('',#13693,1.);
#3723=VECTOR('',#13696,1.);
#3724=VECTOR('',#13699,1.);
#3725=VECTOR('',#13700,1.);
#3726=VECTOR('',#13703,1.);
#3727=VECTOR('',#13704,1.);
#3728=VECTOR('',#13715,1.);
#3729=VECTOR('',#13718,1.);
#3730=VECTOR('',#13723,1.);
#3731=VECTOR('',#13726,1.);
#3732=VECTOR('',#13731,1.);
#3733=VECTOR('',#13732,1.);
#3734=VECTOR('',#13737,1.);
#3735=VECTOR('',#13740,1.);
#3736=VECTOR('',#13745,1.);
#3737=VECTOR('',#13748,1.);
#3738=VECTOR('',#13753,1.);
#3739=VECTOR('',#13754,1.);
#3740=VECTOR('',#13759,1.);
#3741=VECTOR('',#13760,1.);
#3742=VECTOR('',#13761,1.);
#3743=VECTOR('',#13762,1.);
#3744=VECTOR('',#13763,1.);
#3745=VECTOR('',#13764,1.);
#3746=VECTOR('',#13765,1.);
#3747=VECTOR('',#13766,1.);
#3748=VECTOR('',#13767,1.);
#3749=VECTOR('',#13768,1.);
#3750=VECTOR('',#13771,1.);
#3751=VECTOR('',#13772,1.);
#3752=VECTOR('',#13775,1.);
#3753=VECTOR('',#13776,1.);
#3754=VECTOR('',#13779,1.);
#3755=VECTOR('',#13784,0.225);
#3756=VECTOR('',#13789,0.225);
#3757=VECTOR('',#13792,1.);
#3758=VECTOR('',#13793,1.);
#3759=VECTOR('',#13794,1.);
#3760=VECTOR('',#13797,1.);
#3761=VECTOR('',#13798,1.);
#3762=VECTOR('',#13799,1.);
#3763=VECTOR('',#13802,1.);
#3764=VECTOR('',#13805,1.);
#3765=VECTOR('',#13806,1.);
#3766=VECTOR('',#13807,1.);
#3767=VECTOR('',#13808,1.);
#3768=VECTOR('',#13811,1.);
#3769=VECTOR('',#13814,1.);
#3770=VECTOR('',#13823,1.);
#3771=VECTOR('',#13826,1.);
#3772=VECTOR('',#13831,1.);
#3773=VECTOR('',#13834,1.);
#3774=VECTOR('',#13839,1.);
#3775=VECTOR('',#13840,1.);
#3776=VECTOR('',#13845,1.);
#3777=VECTOR('',#13848,1.);
#3778=VECTOR('',#13853,1.);
#3779=VECTOR('',#13856,1.);
#3780=VECTOR('',#13861,1.);
#3781=VECTOR('',#13862,1.);
#3782=VECTOR('',#13867,1.);
#3783=VECTOR('',#13868,1.);
#3784=VECTOR('',#13869,1.);
#3785=VECTOR('',#13870,1.);
#3786=VECTOR('',#13871,1.);
#3787=VECTOR('',#13872,1.);
#3788=VECTOR('',#13873,1.);
#3789=VECTOR('',#13874,1.);
#3790=VECTOR('',#13875,1.);
#3791=VECTOR('',#13876,1.);
#3792=VECTOR('',#13879,1.);
#3793=VECTOR('',#13880,1.);
#3794=VECTOR('',#13883,1.);
#3795=VECTOR('',#13884,1.);
#3796=VECTOR('',#13887,1.);
#3797=VECTOR('',#13892,0.225000000000001);
#3798=VECTOR('',#13897,0.225000000000001);
#3799=VECTOR('',#13900,1.);
#3800=VECTOR('',#13901,1.);
#3801=VECTOR('',#13902,1.);
#3802=VECTOR('',#13905,1.);
#3803=VECTOR('',#13906,1.);
#3804=VECTOR('',#13907,1.);
#3805=VECTOR('',#13910,1.);
#3806=VECTOR('',#13913,1.);
#3807=VECTOR('',#13914,1.);
#3808=VECTOR('',#13915,1.);
#3809=VECTOR('',#13916,1.);
#3810=VECTOR('',#13919,1.);
#3811=VECTOR('',#13922,1.);
#3812=VECTOR('',#13945,0.976185);
#3813=VECTOR('',#13952,0.5);
#3814=VECTOR('',#13957,0.53);
#3815=VECTOR('',#13966,0.976185);
#3816=VECTOR('',#13973,0.53);
#3817=VECTOR('',#13992,1.023815);
#3818=VECTOR('',#14003,1.47);
#3819=VECTOR('',#14008,1.5);
#3820=VECTOR('',#14013,1.47);
#3821=VECTOR('',#14018,1.023815);
#3822=VECTOR('',#14069,1.019052);
#3823=VECTOR('',#14146,0.980948);
#3824=VECTOR('',#14175,1.013815);
#3825=VECTOR('',#14182,0.991185);
#3826=VECTOR('',#14193,1.013815);
#3827=VECTOR('',#14200,0.991185);
#3828=VECTOR('',#14215,1.);
#3829=VECTOR('',#14216,1.);
#3830=VECTOR('',#14217,1.);
#3831=VECTOR('',#14218,1.);
#3832=VECTOR('',#14221,1.);
#3833=VECTOR('',#14222,1.);
#3834=VECTOR('',#14223,1.);
#3835=VECTOR('',#14226,1.);
#3836=VECTOR('',#14227,1.);
#3837=VECTOR('',#14228,1.);
#3838=VECTOR('',#14231,1.);
#3839=VECTOR('',#14232,1.);
#3840=VECTOR('',#14233,1.);
#3841=VECTOR('',#14236,1.);
#3842=VECTOR('',#14237,1.);
#3843=VECTOR('',#14238,1.);
#3844=VECTOR('',#14241,1.);
#3845=VECTOR('',#14242,1.);
#3846=VECTOR('',#14243,1.);
#3847=VECTOR('',#14246,1.);
#3848=VECTOR('',#14247,1.);
#3849=VECTOR('',#14248,1.);
#3850=VECTOR('',#14251,1.);
#3851=VECTOR('',#14252,1.);
#3852=VECTOR('',#14253,1.);
#3853=VECTOR('',#14256,1.);
#3854=VECTOR('',#14257,1.);
#3855=VECTOR('',#14258,1.);
#3856=VECTOR('',#14261,1.);
#3857=VECTOR('',#14262,1.);
#3858=VECTOR('',#14263,1.);
#3859=VECTOR('',#14264,1.);
#3860=VECTOR('',#14267,1.);
#3861=VECTOR('',#14268,1.);
#3862=VECTOR('',#14269,1.);
#3863=VECTOR('',#14272,1.);
#3864=VECTOR('',#14273,1.);
#3865=VECTOR('',#14274,1.);
#3866=VECTOR('',#14277,1.);
#3867=VECTOR('',#14278,1.);
#3868=VECTOR('',#14279,1.);
#3869=VECTOR('',#14282,1.);
#3870=VECTOR('',#14283,1.);
#3871=VECTOR('',#14284,1.);
#3872=VECTOR('',#14287,1.);
#3873=VECTOR('',#14288,1.);
#3874=VECTOR('',#14289,1.);
#3875=VECTOR('',#14292,1.);
#3876=VECTOR('',#14293,1.);
#3877=VECTOR('',#14294,1.);
#3878=VECTOR('',#14297,1.);
#3879=VECTOR('',#14298,1.);
#3880=VECTOR('',#14299,1.);
#3881=VECTOR('',#14302,1.);
#3882=VECTOR('',#14303,1.);
#3883=VECTOR('',#14304,1.);
#3884=VECTOR('',#14307,1.);
#3885=VECTOR('',#14308,1.);
#3886=VECTOR('',#14309,1.);
#3887=VECTOR('',#14310,1.);
#3888=VECTOR('',#14313,1.);
#3889=VECTOR('',#14314,1.);
#3890=VECTOR('',#14315,1.);
#3891=VECTOR('',#14318,1.);
#3892=VECTOR('',#14319,1.);
#3893=VECTOR('',#14320,1.);
#3894=VECTOR('',#14323,1.);
#3895=VECTOR('',#14324,1.);
#3896=VECTOR('',#14325,1.);
#3897=VECTOR('',#14328,1.);
#3898=VECTOR('',#14329,1.);
#3899=VECTOR('',#14330,1.);
#3900=VECTOR('',#14333,1.);
#3901=VECTOR('',#14334,1.);
#3902=VECTOR('',#14335,1.);
#3903=VECTOR('',#14338,1.);
#3904=VECTOR('',#14339,1.);
#3905=VECTOR('',#14340,1.);
#3906=VECTOR('',#14343,1.);
#3907=VECTOR('',#14344,1.);
#3908=VECTOR('',#14345,1.);
#3909=VECTOR('',#14348,1.);
#3910=VECTOR('',#14349,1.);
#3911=VECTOR('',#14350,1.);
#3912=VECTOR('',#14353,1.);
#3913=VECTOR('',#14354,1.);
#3914=VECTOR('',#14355,1.);
#3915=VECTOR('',#14356,1.);
#3916=VECTOR('',#14359,1.);
#3917=VECTOR('',#14360,1.);
#3918=VECTOR('',#14361,1.);
#3919=VECTOR('',#14364,1.);
#3920=VECTOR('',#14365,1.);
#3921=VECTOR('',#14366,1.);
#3922=VECTOR('',#14369,1.);
#3923=VECTOR('',#14370,1.);
#3924=VECTOR('',#14371,1.);
#3925=VECTOR('',#14374,1.);
#3926=VECTOR('',#14375,1.);
#3927=VECTOR('',#14376,1.);
#3928=VECTOR('',#14379,1.);
#3929=VECTOR('',#14380,1.);
#3930=VECTOR('',#14381,1.);
#3931=VECTOR('',#14384,1.);
#3932=VECTOR('',#14385,1.);
#3933=VECTOR('',#14386,1.);
#3934=VECTOR('',#14389,1.);
#3935=VECTOR('',#14390,1.);
#3936=VECTOR('',#14391,1.);
#3937=VECTOR('',#14394,1.);
#3938=VECTOR('',#14395,1.);
#3939=VECTOR('',#14396,1.);
#3940=VECTOR('',#14401,0.21);
#3941=VECTOR('',#14406,1.);
#3942=VECTOR('',#14407,1.);
#3943=VECTOR('',#14408,1.);
#3944=VECTOR('',#14411,1.);
#3945=VECTOR('',#14412,1.);
#3946=VECTOR('',#14413,1.);
#3947=VECTOR('',#14416,1.);
#3948=VECTOR('',#14417,1.);
#3949=VECTOR('',#14420,1.);
#3950=VECTOR('',#14421,1.);
#3951=VECTOR('',#14422,1.);
#3952=VECTOR('',#14425,1.);
#3953=VECTOR('',#14426,1.);
#3954=VECTOR('',#14429,1.);
#3955=VECTOR('',#14430,1.);
#3956=VECTOR('',#14431,1.);
#3957=VECTOR('',#14434,1.);
#3958=VECTOR('',#14435,1.);
#3959=VECTOR('',#14438,1.);
#3960=VECTOR('',#14439,1.);
#3961=VECTOR('',#14448,1.);
#3962=VECTOR('',#14449,1.);
#3963=VECTOR('',#14450,1.);
#3964=VECTOR('',#14451,1.);
#3965=VECTOR('',#14454,1.);
#3966=VECTOR('',#14455,1.);
#3967=VECTOR('',#14456,1.);
#3968=VECTOR('',#14459,1.);
#3969=VECTOR('',#14460,1.);
#3970=VECTOR('',#14461,1.);
#3971=VECTOR('',#14466,1.);
#3972=VECTOR('',#14467,1.);
#3973=VECTOR('',#14468,1.);
#3974=VECTOR('',#14469,1.);
#3975=VECTOR('',#14470,1.);
#3976=VECTOR('',#14471,1.);
#3977=VECTOR('',#14472,1.);
#3978=VECTOR('',#14475,1.);
#3979=VECTOR('',#14476,1.);
#3980=VECTOR('',#14479,1.);
#3981=VECTOR('',#14480,1.);
#3982=VECTOR('',#14483,1.);
#3983=VECTOR('',#14484,1.);
#3984=VECTOR('',#14485,1.);
#3985=VECTOR('',#14486,1.);
#3986=VECTOR('',#14487,1.);
#3987=VECTOR('',#14490,1.);
#3988=VECTOR('',#14493,1.);
#3989=VECTOR('',#14496,1.);
#3990=VECTOR('',#14501,0.21);
#3991=VECTOR('',#14510,1.);
#3992=VECTOR('',#14513,1.);
#3993=VECTOR('',#14516,1.);
#3994=VECTOR('',#14523,1.);
#3995=VECTOR('',#14524,1.);
#3996=VECTOR('',#14525,1.);
#3997=VECTOR('',#14526,1.);
#3998=VECTOR('',#14529,1.);
#3999=VECTOR('',#14530,1.);
#4000=VECTOR('',#14531,1.);
#4001=VECTOR('',#14534,1.);
#4002=VECTOR('',#14535,1.);
#4003=VECTOR('',#14536,1.);
#4004=VECTOR('',#14539,1.);
#4005=VECTOR('',#14540,1.);
#4006=VECTOR('',#14541,1.);
#4007=VECTOR('',#14544,1.);
#4008=VECTOR('',#14545,1.);
#4009=VECTOR('',#14546,1.);
#4010=VECTOR('',#14549,1.);
#4011=VECTOR('',#14550,1.);
#4012=VECTOR('',#14567,0.4);
#4013=VECTOR('',#14572,0.425);
#4014=VECTOR('',#14577,0.41);
#4015=VECTOR('',#14586,0.26);
#4016=VECTOR('',#14589,0.25);
#4017=VECTOR('',#14596,0.375);
#4018=VECTOR('',#14607,0.375);
#4019=VECTOR('',#14618,0.375);
#4020=VECTOR('',#14629,0.375);
#4021=VECTOR('',#14640,0.225);
#4022=VECTOR('',#14645,0.225);
#4023=VECTOR('',#14650,0.225);
#4024=VECTOR('',#14655,0.225000000000001);
#4025=VECTOR('',#14658,1.);
#4026=VECTOR('',#14659,1.);
#4027=VECTOR('',#14660,1.);
#4028=VECTOR('',#14661,1.);
#4029=VECTOR('',#14664,1.);
#4030=VECTOR('',#14665,1.);
#4031=VECTOR('',#14666,1.);
#4032=VECTOR('',#14669,1.);
#4033=VECTOR('',#14670,1.);
#4034=VECTOR('',#14671,1.);
#4035=VECTOR('',#14674,1.);
#4036=VECTOR('',#14675,1.);
#4037=VECTOR('',#14676,1.);
#4038=VECTOR('',#14679,1.);
#4039=VECTOR('',#14680,1.);
#4040=VECTOR('',#14681,1.);
#4041=VECTOR('',#14684,1.);
#4042=VECTOR('',#14685,1.);
#4043=VECTOR('',#14686,1.);
#4044=VECTOR('',#14689,1.);
#4045=VECTOR('',#14690,1.);
#4046=VECTOR('',#14691,1.);
#4047=VECTOR('',#14694,1.);
#4048=VECTOR('',#14695,1.);
#4049=VECTOR('',#14696,1.);
#4050=VECTOR('',#14699,1.);
#4051=VECTOR('',#14700,1.);
#4052=VECTOR('',#14701,1.);
#4053=VECTOR('',#14704,1.);
#4054=VECTOR('',#14705,1.);
#4055=VECTOR('',#14706,1.);
#4056=VECTOR('',#14709,1.);
#4057=VECTOR('',#14710,1.);
#4058=VECTOR('',#14711,1.);
#4059=VECTOR('',#14714,1.);
#4060=VECTOR('',#14715,1.);
#4061=VECTOR('',#14728,0.165);
#4062=VECTOR('',#14747,0.7);
#4063=VECTOR('',#14750,0.5);
#4064=VECTOR('',#14757,0.4);
#4065=VECTOR('',#14766,0.5);
#4066=VECTOR('',#14777,0.505);
#4067=VECTOR('',#14786,0.405);
#4068=VECTOR('',#14793,0.7);
#4069=VECTOR('',#14806,0.505);
#4070=VECTOR('',#14813,0.7);
#4071=VECTOR('',#14826,0.15);
#4072=VECTOR('',#14839,0.15);
#4073=VECTOR('',#14852,0.225);
#4074=VECTOR('',#14859,0.6);
#4075=VECTOR('',#14874,0.164999999999999);
#4076=VECTOR('',#14893,0.700000000000003);
#4077=VECTOR('',#14896,0.5);
#4078=VECTOR('',#14903,0.399999999999999);
#4079=VECTOR('',#14912,0.5);
#4080=VECTOR('',#14923,0.505000000000003);
#4081=VECTOR('',#14932,0.405000000000001);
#4082=VECTOR('',#14939,0.700000000000003);
#4083=VECTOR('',#14952,0.505000000000003);
#4084=VECTOR('',#14959,0.700000000000003);
#4085=VECTOR('',#14972,0.149999999999999);
#4086=VECTOR('',#14985,0.149999999999999);
#4087=VECTOR('',#14998,0.225000000000001);
#4088=VECTOR('',#15005,0.600000000000001);
#4089=VECTOR('',#15016,0.125);
#4090=VECTOR('',#15019,0.125);
#4091=VECTOR('',#15024,0.65);
#4092=VECTOR('',#15025,0.65);
#4093=VECTOR('',#15030,0.125);
#4094=VECTOR('',#15033,0.125);
#4095=VECTOR('',#15038,0.4);
#4096=VECTOR('',#15039,0.4);
#4097=VECTOR('',#15132,0.8);
#4098=VECTOR('',#15223,0.8);
#4099=VECTOR('',#15228,1.);
#4100=VECTOR('',#15229,1.);
#4101=VECTOR('',#15232,1.);
#4102=VECTOR('',#15235,1.);
#4103=VECTOR('',#15238,1.);
#4104=VECTOR('',#15241,1.);
#4105=VECTOR('',#15244,1.);
#4106=VECTOR('',#15247,1.);
#4107=VECTOR('',#15250,1.);
#4108=VECTOR('',#15253,1.);
#4109=VECTOR('',#15256,1.);
#4110=VECTOR('',#15259,1.);
#4111=VECTOR('',#15262,1.);
#4112=VECTOR('',#15265,1.);
#4113=VECTOR('',#15268,1.);
#4114=VECTOR('',#15271,1.);
#4115=VECTOR('',#15274,1.);
#4116=VECTOR('',#15277,1.);
#4117=VECTOR('',#15280,1.);
#4118=VECTOR('',#15283,1.);
#4119=VECTOR('',#15286,1.);
#4120=VECTOR('',#15289,1.);
#4121=VECTOR('',#15292,1.);
#4122=VECTOR('',#15295,1.);
#4123=VECTOR('',#15298,1.);
#4124=VECTOR('',#15301,1.);
#4125=VECTOR('',#15304,1.);
#4126=VECTOR('',#15307,1.);
#4127=VECTOR('',#15310,1.);
#4128=VECTOR('',#15313,1.);
#4129=VECTOR('',#15316,1.);
#4130=VECTOR('',#15319,1.);
#4131=VECTOR('',#15322,1.);
#4132=VECTOR('',#15325,1.);
#4133=VECTOR('',#15328,1.);
#4134=VECTOR('',#15331,1.);
#4135=VECTOR('',#15334,1.);
#4136=VECTOR('',#15337,1.);
#4137=VECTOR('',#15340,1.);
#4138=VECTOR('',#15343,1.);
#4139=VECTOR('',#15354,0.4);
#4140=VECTOR('',#15365,0.399999999999999);
#4141=VECTOR('',#15374,0.225);
#4142=VECTOR('',#15379,0.225000000000001);
#4143=VECTOR('',#15386,0.274999999999999);
#4144=VECTOR('',#15393,0.275);
#4145=VECTOR('',#15400,0.275);
#4146=VECTOR('',#15407,0.274999999999999);
#4147=VECTOR('',#15412,1.);
#4148=VECTOR('',#15413,1.);
#4149=VECTOR('',#15414,1.);
#4150=VECTOR('',#15415,1.);
#4151=VECTOR('',#15418,1.);
#4152=VECTOR('',#15419,1.);
#4153=VECTOR('',#15420,1.);
#4154=VECTOR('',#15423,1.);
#4155=VECTOR('',#15424,1.);
#4156=VECTOR('',#15425,1.);
#4157=VECTOR('',#15428,1.);
#4158=VECTOR('',#15429,1.);
#4159=VECTOR('',#15440,0.164999999999999);
#4160=VECTOR('',#15449,0.164999999999999);
#4161=VECTOR('',#15456,1.);
#4162=VECTOR('',#15459,1.);
#4163=VECTOR('',#15460,1.);
#4164=VECTOR('',#15463,1.);
#4165=VECTOR('',#15466,1.);
#4166=VECTOR('',#15469,1.);
#4167=VECTOR('',#15472,1.);
#4168=VECTOR('',#15477,1.);
#4169=VECTOR('',#15478,1.);
#4170=VECTOR('',#15479,1.);
#4171=VECTOR('',#15482,1.);
#4172=VECTOR('',#15483,1.);
#4173=VECTOR('',#15484,1.);
#4174=VECTOR('',#15485,1.);
#4175=VECTOR('',#15486,1.);
#4176=VECTOR('',#15489,1.);
#4177=VECTOR('',#15490,1.);
#4178=VECTOR('',#15491,1.);
#4179=VECTOR('',#15496,0.164999999999999);
#4180=VECTOR('',#15505,0.164999999999999);
#4181=VECTOR('',#15512,1.);
#4182=VECTOR('',#15513,1.);
#4183=VECTOR('',#15514,1.);
#4184=VECTOR('',#15517,1.);
#4185=VECTOR('',#15518,1.);
#4186=VECTOR('',#15521,1.);
#4187=VECTOR('',#15524,1.);
#4188=VECTOR('',#15525,1.);
#4189=VECTOR('',#15534,1.);
#4190=VECTOR('',#15535,1.);
#4191=VECTOR('',#15536,1.);
#4192=VECTOR('',#15537,1.);
#4193=VECTOR('',#15540,1.);
#4194=VECTOR('',#15541,1.);
#4195=VECTOR('',#15542,1.);
#4196=VECTOR('',#15545,1.);
#4197=VECTOR('',#15546,1.);
#4198=VECTOR('',#15547,1.);
#4199=VECTOR('',#15550,1.);
#4200=VECTOR('',#15551,1.);
#4201=VECTOR('',#15562,1.);
#4202=VECTOR('',#15567,1.);
#4203=VECTOR('',#15570,0.21);
#4204=VECTOR('',#15575,1.);
#4205=VECTOR('',#15578,1.);
#4206=VECTOR('',#15583,1.);
#4207=VECTOR('',#15586,0.21);
#4208=VECTOR('',#15591,1.);
#4209=VECTOR('',#15594,1.);
#4210=VECTOR('',#15599,1.);
#4211=VECTOR('',#15602,0.21);
#4212=VECTOR('',#15607,1.);
#4213=VECTOR('',#15610,1.);
#4214=VECTOR('',#15615,1.);
#4215=VECTOR('',#15618,0.21);
#4216=VECTOR('',#15623,1.);
#4217=VECTOR('',#15626,1.);
#4218=VECTOR('',#15627,1.);
#4219=VECTOR('',#15628,1.);
#4220=VECTOR('',#15629,1.);
#4221=VECTOR('',#15630,1.);
#4222=VECTOR('',#15631,1.);
#4223=VECTOR('',#15634,1.);
#4224=VECTOR('',#15635,1.);
#4225=VECTOR('',#15636,1.);
#4226=VECTOR('',#15637,1.);
#4227=VECTOR('',#15638,1.);
#4228=VECTOR('',#15639,1.);
#4229=VECTOR('',#15642,1.);
#4230=VECTOR('',#15643,1.);
#4231=VECTOR('',#15644,1.);
#4232=VECTOR('',#15645,1.);
#4233=VECTOR('',#15646,1.);
#4234=VECTOR('',#15647,1.);
#4235=VECTOR('',#15648,1.);
#4236=VECTOR('',#15649,1.);
#4237=VECTOR('',#15650,1.);
#4238=VECTOR('',#15651,1.);
#4239=VECTOR('',#15654,1.);
#4240=VECTOR('',#15655,1.);
#4241=VECTOR('',#15658,1.);
#4242=VECTOR('',#15659,1.);
#4243=VECTOR('',#15662,1.);
#4244=VECTOR('',#15663,1.);
#4245=VECTOR('',#15666,1.);
#4246=VECTOR('',#15667,1.);
#4247=VECTOR('',#15670,1.);
#4248=VECTOR('',#15673,1.);
#4249=VECTOR('',#15674,1.);
#4250=VECTOR('',#15677,1.);
#4251=VECTOR('',#15678,1.);
#4252=VECTOR('',#15681,1.);
#4253=VECTOR('',#15682,1.);
#4254=VECTOR('',#15685,1.);
#4255=VECTOR('',#15686,1.);
#4256=VECTOR('',#15689,1.);
#4257=VECTOR('',#15696,1.);
#4258=VECTOR('',#15697,1.);
#4259=VECTOR('',#15698,1.);
#4260=VECTOR('',#15699,1.);
#4261=VECTOR('',#15702,1.);
#4262=VECTOR('',#15703,1.);
#4263=VECTOR('',#15704,1.);
#4264=VECTOR('',#15707,1.);
#4265=VECTOR('',#15708,1.);
#4266=VECTOR('',#15709,1.);
#4267=VECTOR('',#15712,1.);
#4268=VECTOR('',#15713,1.);
#4269=VECTOR('',#15714,1.);
#4270=VECTOR('',#15717,1.);
#4271=VECTOR('',#15718,1.);
#4272=VECTOR('',#15719,1.);
#4273=VECTOR('',#15722,1.);
#4274=VECTOR('',#15723,1.);
#4275=VECTOR('',#15724,1.);
#4276=VECTOR('',#15727,1.);
#4277=VECTOR('',#15728,1.);
#4278=VECTOR('',#15729,1.);
#4279=VECTOR('',#15732,1.);
#4280=VECTOR('',#15733,1.);
#4281=VECTOR('',#15742,1.);
#4282=VECTOR('',#15743,1.);
#4283=VECTOR('',#15744,1.);
#4284=VECTOR('',#15745,1.);
#4285=VECTOR('',#15748,1.);
#4286=VECTOR('',#15749,1.);
#4287=VECTOR('',#15750,1.);
#4288=VECTOR('',#15753,1.);
#4289=VECTOR('',#15754,1.);
#4290=VECTOR('',#15755,1.);
#4291=VECTOR('',#15758,1.);
#4292=VECTOR('',#15759,1.);
#4293=VECTOR('',#15760,1.);
#4294=VECTOR('',#15763,1.);
#4295=VECTOR('',#15764,1.);
#4296=VECTOR('',#15765,1.);
#4297=VECTOR('',#15768,1.);
#4298=VECTOR('',#15769,1.);
#4299=VECTOR('',#15770,1.);
#4300=VECTOR('',#15773,1.);
#4301=VECTOR('',#15774,1.);
#4302=VECTOR('',#15775,1.);
#4303=VECTOR('',#15778,1.);
#4304=VECTOR('',#15779,1.);
#4305=VECTOR('',#15796,0.275);
#4306=VECTOR('',#15801,0.265);
#4307=VECTOR('',#15810,0.5);
#4308=VECTOR('',#15825,0.4);
#4309=VECTOR('',#15830,0.425);
#4310=VECTOR('',#15835,0.41);
#4311=VECTOR('',#15844,0.26);
#4312=VECTOR('',#15849,0.25);
#4313=VECTOR('',#15854,0.225);
#4314=VECTOR('',#15859,1.);
#4315=VECTOR('',#15860,1.);
#4316=VECTOR('',#15861,1.);
#4317=VECTOR('',#15862,1.);
#4318=VECTOR('',#15865,1.);
#4319=VECTOR('',#15866,1.);
#4320=VECTOR('',#15867,1.);
#4321=VECTOR('',#15870,1.);
#4322=VECTOR('',#15871,1.);
#4323=VECTOR('',#15872,1.);
#4324=VECTOR('',#15875,1.);
#4325=VECTOR('',#15876,1.);
#4326=VECTOR('',#15877,1.);
#4327=VECTOR('',#15880,1.);
#4328=VECTOR('',#15881,1.);
#4329=VECTOR('',#15882,1.);
#4330=VECTOR('',#15885,1.);
#4331=VECTOR('',#15886,1.);
#4332=VECTOR('',#15895,1.);
#4333=VECTOR('',#15896,1.);
#4334=VECTOR('',#15897,1.);
#4335=VECTOR('',#15898,1.);
#4336=VECTOR('',#15901,1.);
#4337=VECTOR('',#15902,1.);
#4338=VECTOR('',#15903,1.);
#4339=VECTOR('',#15906,1.);
#4340=VECTOR('',#15907,1.);
#4341=VECTOR('',#15908,1.);
#4342=VECTOR('',#15911,1.);
#4343=VECTOR('',#15912,1.);
#4344=VECTOR('',#15913,1.);
#4345=VECTOR('',#15916,1.);
#4346=VECTOR('',#15917,1.);
#4347=VECTOR('',#15918,1.);
#4348=VECTOR('',#15921,1.);
#4349=VECTOR('',#15922,1.);
#4350=VECTOR('',#15939,0.325);
#4351=VECTOR('',#15944,0.35);
#4352=VECTOR('',#15949,0.335);
#4353=VECTOR('',#15958,0.21);
#4354=VECTOR('',#15961,0.2);
#4355=VECTOR('',#15972,0.325);
#4356=VECTOR('',#15977,0.35);
#4357=VECTOR('',#15982,0.335);
#4358=VECTOR('',#15991,0.21);
#4359=VECTOR('',#15996,0.2);
#4360=VECTOR('',#16001,0.18);
#4361=VECTOR('',#16006,1.);
#4362=VECTOR('',#16007,1.);
#4363=VECTOR('',#16008,1.);
#4364=VECTOR('',#16009,1.);
#4365=VECTOR('',#16012,1.);
#4366=VECTOR('',#16013,1.);
#4367=VECTOR('',#16014,1.);
#4368=VECTOR('',#16017,1.);
#4369=VECTOR('',#16018,1.);
#4370=VECTOR('',#16019,1.);
#4371=VECTOR('',#16022,1.);
#4372=VECTOR('',#16023,1.);
#4373=VECTOR('',#16024,1.);
#4374=VECTOR('',#16027,1.);
#4375=VECTOR('',#16028,1.);
#4376=VECTOR('',#16029,1.);
#4377=VECTOR('',#16032,1.);
#4378=VECTOR('',#16033,1.);
#4379=CIRCLE('',#11494,0.164999999999999);
#4380=CIRCLE('',#11495,0.164999999999999);
#4381=CIRCLE('',#11498,0.164999999999999);
#4382=CIRCLE('',#11499,0.164999999999999);
#4383=CIRCLE('',#11502,0.165);
#4384=CIRCLE('',#11503,0.165);
#4385=CIRCLE('',#11506,0.165);
#4386=CIRCLE('',#11507,0.165);
#4387=CIRCLE('',#11510,0.164999999999999);
#4388=CIRCLE('',#11511,0.164999999999999);
#4389=CIRCLE('',#11514,0.164999999999999);
#4390=CIRCLE('',#11515,0.164999999999999);
#4391=CIRCLE('',#11518,0.164999999999999);
#4392=CIRCLE('',#11519,0.164999999999999);
#4393=CIRCLE('',#11522,0.165);
#4394=CIRCLE('',#11523,0.165);
#4395=CIRCLE('',#11526,0.274999999999999);
#4396=CIRCLE('',#11527,0.274999999999999);
#4397=CIRCLE('',#11529,0.275);
#4398=CIRCLE('',#11530,0.275);
#4399=CIRCLE('',#11532,0.274999999999999);
#4400=CIRCLE('',#11533,0.274999999999999);
#4401=CIRCLE('',#11535,0.275);
#4402=CIRCLE('',#11536,0.275);
#4403=CIRCLE('',#11538,0.164999999999999);
#4404=CIRCLE('',#11539,0.164999999999999);
#4405=CIRCLE('',#11542,0.164999999999999);
#4406=CIRCLE('',#11543,0.164999999999999);
#4407=CIRCLE('',#11546,0.164999999999999);
#4408=CIRCLE('',#11547,0.164999999999999);
#4409=CIRCLE('',#11550,0.164999999999999);
#4410=CIRCLE('',#11551,0.164999999999999);
#4411=CIRCLE('',#11554,0.165);
#4412=CIRCLE('',#11555,0.165);
#4413=CIRCLE('',#11558,0.165);
#4414=CIRCLE('',#11559,0.165);
#4415=CIRCLE('',#11562,0.165);
#4416=CIRCLE('',#11563,0.165);
#4417=CIRCLE('',#11566,0.165);
#4418=CIRCLE('',#11567,0.165);
#4419=CIRCLE('',#11603,0.165);
#4420=CIRCLE('',#11604,0.165);
#4421=CIRCLE('',#11606,0.165);
#4422=CIRCLE('',#11607,0.165);
#4423=CIRCLE('',#11609,0.165);
#4424=CIRCLE('',#11610,0.165);
#4425=CIRCLE('',#11612,0.165);
#4426=CIRCLE('',#11613,0.165);
#4427=CIRCLE('',#11615,1.5);
#4428=CIRCLE('',#11616,1.5);
#4429=CIRCLE('',#11618,0.225);
#4430=CIRCLE('',#11619,0.225);
#4431=CIRCLE('',#11621,0.225);
#4432=CIRCLE('',#11622,0.225);
#4433=CIRCLE('',#11624,0.225);
#4434=CIRCLE('',#11625,0.225);
#4435=CIRCLE('',#11627,0.225);
#4436=CIRCLE('',#11628,0.225);
#4437=CIRCLE('',#11641,1.1);
#4438=CIRCLE('',#11642,1.1);
#4439=CIRCLE('',#11644,1.49);
#4440=CIRCLE('',#11645,1.49);
#4441=CIRCLE('',#11650,0.225);
#4442=CIRCLE('',#11651,0.225);
#4443=CIRCLE('',#11653,0.225);
#4444=CIRCLE('',#11654,0.225);
#4445=CIRCLE('',#11656,0.225);
#4446=CIRCLE('',#11657,0.225);
#4447=CIRCLE('',#11659,0.225);
#4448=CIRCLE('',#11660,0.225);
#4449=CIRCLE('',#11662,2.1);
#4450=CIRCLE('',#11663,2.1);
#4451=CIRCLE('',#11664,2.1);
#4452=CIRCLE('',#11665,2.1);
#4453=CIRCLE('',#11666,1.1);
#4454=CIRCLE('',#11668,2.1);
#4455=CIRCLE('',#11670,2.1);
#4456=CIRCLE('',#11672,2.1);
#4457=CIRCLE('',#11674,2.1);
#4458=CIRCLE('',#11676,1.49);
#4459=CIRCLE('',#11677,1.49);
#4460=CIRCLE('',#11679,1.1);
#4461=CIRCLE('',#11684,0.225);
#4462=CIRCLE('',#11685,0.225);
#4463=CIRCLE('',#11687,0.225);
#4464=CIRCLE('',#11688,0.225);
#4465=CIRCLE('',#11690,0.225);
#4466=CIRCLE('',#11691,0.225);
#4467=CIRCLE('',#11693,0.225);
#4468=CIRCLE('',#11694,0.225);
#4469=CIRCLE('',#11696,2.1);
#4470=CIRCLE('',#11697,2.1);
#4471=CIRCLE('',#11698,2.1);
#4472=CIRCLE('',#11699,2.1);
#4473=CIRCLE('',#11700,1.49);
#4474=CIRCLE('',#11702,2.1);
#4475=CIRCLE('',#11704,2.1);
#4476=CIRCLE('',#11706,2.1);
#4477=CIRCLE('',#11708,2.1);
#4478=CIRCLE('',#11710,1.49);
#4479=CIRCLE('',#11712,1.1);
#4480=CIRCLE('',#11714,1.1);
#4481=CIRCLE('',#11718,0.164999999999999);
#4482=CIRCLE('',#11719,0.164999999999999);
#4483=CIRCLE('',#11721,0.164999999999999);
#4484=CIRCLE('',#11722,0.164999999999999);
#4485=CIRCLE('',#11724,0.164999999999999);
#4486=CIRCLE('',#11725,0.164999999999999);
#4487=CIRCLE('',#11727,0.164999999999999);
#4488=CIRCLE('',#11728,0.164999999999999);
#4489=CIRCLE('',#11730,1.5);
#4490=CIRCLE('',#11731,1.5);
#4491=CIRCLE('',#11733,0.225000000000001);
#4492=CIRCLE('',#11734,0.225000000000001);
#4493=CIRCLE('',#11736,0.225000000000001);
#4494=CIRCLE('',#11737,0.225000000000001);
#4495=CIRCLE('',#11739,0.225000000000001);
#4496=CIRCLE('',#11740,0.225000000000001);
#4497=CIRCLE('',#11742,0.225000000000001);
#4498=CIRCLE('',#11743,0.225000000000001);
#4499=CIRCLE('',#11756,1.1);
#4500=CIRCLE('',#11757,1.1);
#4501=CIRCLE('',#11759,1.49);
#4502=CIRCLE('',#11760,1.49);
#4503=CIRCLE('',#11765,0.225000000000001);
#4504=CIRCLE('',#11766,0.225000000000001);
#4505=CIRCLE('',#11768,0.225000000000001);
#4506=CIRCLE('',#11769,0.225000000000001);
#4507=CIRCLE('',#11771,0.225000000000001);
#4508=CIRCLE('',#11772,0.225000000000001);
#4509=CIRCLE('',#11774,0.225000000000001);
#4510=CIRCLE('',#11775,0.225000000000001);
#4511=CIRCLE('',#11777,2.1);
#4512=CIRCLE('',#11778,2.1);
#4513=CIRCLE('',#11779,2.1);
#4514=CIRCLE('',#11780,2.1);
#4515=CIRCLE('',#11781,1.1);
#4516=CIRCLE('',#11783,2.1);
#4517=CIRCLE('',#11785,2.1);
#4518=CIRCLE('',#11787,2.1);
#4519=CIRCLE('',#11789,2.1);
#4520=CIRCLE('',#11791,1.49);
#4521=CIRCLE('',#11792,1.49);
#4522=CIRCLE('',#11794,1.1);
#4523=CIRCLE('',#11799,0.225000000000001);
#4524=CIRCLE('',#11800,0.225000000000001);
#4525=CIRCLE('',#11802,0.225000000000001);
#4526=CIRCLE('',#11803,0.225000000000001);
#4527=CIRCLE('',#11805,0.225000000000001);
#4528=CIRCLE('',#11806,0.225000000000001);
#4529=CIRCLE('',#11808,0.225000000000001);
#4530=CIRCLE('',#11809,0.225000000000001);
#4531=CIRCLE('',#11811,2.1);
#4532=CIRCLE('',#11812,2.1);
#4533=CIRCLE('',#11813,2.1);
#4534=CIRCLE('',#11814,2.1);
#4535=CIRCLE('',#11815,1.49);
#4536=CIRCLE('',#11817,2.1);
#4537=CIRCLE('',#11819,2.1);
#4538=CIRCLE('',#11821,2.1);
#4539=CIRCLE('',#11823,2.1);
#4540=CIRCLE('',#11825,1.49);
#4541=CIRCLE('',#11827,1.1);
#4542=CIRCLE('',#11829,1.1);
#4543=CIRCLE('',#11835,0.736619772367581);
#4544=CIRCLE('',#11836,0.736619772367582);
#4545=CIRCLE('',#11837,0.636619772367581);
#4546=CIRCLE('',#11838,0.636619772367581);
#4547=CIRCLE('',#11840,0.636619772367581);
#4548=CIRCLE('',#11842,0.636619772367581);
#4549=CIRCLE('',#11844,0.736619772367582);
#4550=CIRCLE('',#11848,0.736619772367581);
#4551=CIRCLE('',#11852,0.4);
#4552=CIRCLE('',#11853,0.4);
#4553=CIRCLE('',#11855,0.4);
#4554=CIRCLE('',#11856,0.4);
#4555=CIRCLE('',#11858,0.225);
#4556=CIRCLE('',#11860,0.4);
#4557=CIRCLE('',#11861,0.4);
#4558=CIRCLE('',#11863,0.4);
#4559=CIRCLE('',#11864,0.4);
#4560=CIRCLE('',#11866,0.225);
#4561=CIRCLE('',#11872,0.225);
#4562=CIRCLE('',#11874,0.225);
#4563=CIRCLE('',#11885,0.399999999999999);
#4564=CIRCLE('',#11886,0.399999999999999);
#4565=CIRCLE('',#11888,0.399999999999999);
#4566=CIRCLE('',#11889,0.399999999999999);
#4567=CIRCLE('',#11891,0.225000000000001);
#4568=CIRCLE('',#11893,0.399999999999999);
#4569=CIRCLE('',#11894,0.399999999999999);
#4570=CIRCLE('',#11896,0.399999999999999);
#4571=CIRCLE('',#11897,0.399999999999999);
#4572=CIRCLE('',#11899,0.225000000000001);
#4573=CIRCLE('',#11905,0.225000000000001);
#4574=CIRCLE('',#11907,0.225000000000001);
#4575=CIRCLE('',#11919,0.976185);
#4576=CIRCLE('',#11920,0.976185);
#4577=CIRCLE('',#11921,0.247676);
#4578=CIRCLE('',#11922,0.976185);
#4579=CIRCLE('',#11923,0.976185);
#4580=CIRCLE('',#11925,0.976185);
#4581=CIRCLE('',#11927,0.5);
#4582=CIRCLE('',#11928,0.5);
#4583=CIRCLE('',#11930,0.56);
#4584=CIRCLE('',#11933,0.976185);
#4585=CIRCLE('',#11935,0.56);
#4586=CIRCLE('',#11939,1.023815);
#4587=CIRCLE('',#11940,1.023815);
#4588=CIRCLE('',#11941,0.247676);
#4589=CIRCLE('',#11942,1.023815);
#4590=CIRCLE('',#11943,1.023815);
#4591=CIRCLE('',#11945,1.023815);
#4592=CIRCLE('',#11947,1.44);
#4593=CIRCLE('',#11948,1.023815);
#4594=CIRCLE('',#11950,1.5);
#4595=CIRCLE('',#11952,1.5);
#4596=CIRCLE('',#11954,1.44);
#4597=CIRCLE('',#11959,0.23815);
#4598=CIRCLE('',#11961,0.23815);
#4599=CIRCLE('',#11963,0.23815);
#4600=CIRCLE('',#11965,0.23815);
#4601=CIRCLE('',#11967,0.23815);
#4602=CIRCLE('',#11969,0.23815);
#4603=CIRCLE('',#11971,0.23815);
#4604=CIRCLE('',#11973,0.23815);
#4605=CIRCLE('',#11976,0.243053047864041);
#4606=CIRCLE('',#11977,0.243053047864041);
#4607=CIRCLE('',#11979,1.019052);
#4608=CIRCLE('',#11980,1.019052);
#4609=CIRCLE('',#11981,1.019052);
#4610=CIRCLE('',#11982,1.019052);
#4611=CIRCLE('',#11983,1.019052);
#4612=CIRCLE('',#11984,1.019052);
#4613=CIRCLE('',#11985,1.019052);
#4614=CIRCLE('',#11986,1.019052);
#4615=CIRCLE('',#11987,1.019052);
#4616=CIRCLE('',#11989,0.980948);
#4617=CIRCLE('',#11990,0.243053047864041);
#4618=CIRCLE('',#11992,0.243053047864041);
#4619=CIRCLE('',#11994,0.980948);
#4620=CIRCLE('',#11995,0.243053047864041);
#4621=CIRCLE('',#11997,0.243053047864041);
#4622=CIRCLE('',#11999,0.980948);
#4623=CIRCLE('',#12000,0.243053047864041);
#4624=CIRCLE('',#12002,0.243053047864041);
#4625=CIRCLE('',#12004,0.980948);
#4626=CIRCLE('',#12005,0.243053047864041);
#4627=CIRCLE('',#12007,0.243053047864041);
#4628=CIRCLE('',#12009,0.980948);
#4629=CIRCLE('',#12010,0.243053047864041);
#4630=CIRCLE('',#12012,0.243053047864041);
#4631=CIRCLE('',#12014,0.980948);
#4632=CIRCLE('',#12015,0.243053047864041);
#4633=CIRCLE('',#12017,0.243053047864041);
#4634=CIRCLE('',#12019,0.980948);
#4635=CIRCLE('',#12020,0.980948);
#4636=CIRCLE('',#12021,0.980948);
#4637=CIRCLE('',#12023,0.243053047864041);
#4638=CIRCLE('',#12025,0.243053047864041);
#4639=CIRCLE('',#12030,1.013815);
#4640=CIRCLE('',#12031,0.991185);
#4641=CIRCLE('',#12033,1.013815);
#4642=CIRCLE('',#12035,0.991185);
#4643=CIRCLE('',#12038,1.013815);
#4644=CIRCLE('',#12039,0.991185);
#4645=CIRCLE('',#12041,1.013815);
#4646=CIRCLE('',#12043,0.991185);
#4647=CIRCLE('',#12088,0.21);
#4648=CIRCLE('',#12089,0.21);
#4649=CIRCLE('',#12104,0.2117);
#4650=CIRCLE('',#12113,0.2117);
#4651=CIRCLE('',#12114,0.2117);
#4652=CIRCLE('',#12116,0.2117);
#4653=CIRCLE('',#12131,0.24505);
#4654=CIRCLE('',#12133,0.375);
#4655=CIRCLE('',#12135,0.425);
#4656=CIRCLE('',#12137,0.425);
#4657=CIRCLE('',#12139,0.395);
#4658=CIRCLE('',#12141,0.27);
#4659=CIRCLE('',#12143,0.24505);
#4660=CIRCLE('',#12147,0.375);
#4661=CIRCLE('',#12148,0.375);
#4662=CIRCLE('',#12150,0.225);
#4663=CIRCLE('',#12152,0.375);
#4664=CIRCLE('',#12153,0.375);
#4665=CIRCLE('',#12155,0.225);
#4666=CIRCLE('',#12157,0.375);
#4667=CIRCLE('',#12158,0.375);
#4668=CIRCLE('',#12160,0.225);
#4669=CIRCLE('',#12162,0.375);
#4670=CIRCLE('',#12163,0.375);
#4671=CIRCLE('',#12165,0.225000000000001);
#4672=CIRCLE('',#12167,0.225);
#4673=CIRCLE('',#12169,0.225);
#4674=CIRCLE('',#12171,0.225);
#4675=CIRCLE('',#12173,0.225000000000001);
#4676=CIRCLE('',#12191,0.165);
#4677=CIRCLE('',#12192,0.165);
#4678=CIRCLE('',#12195,0.7);
#4679=CIRCLE('',#12196,0.5);
#4680=CIRCLE('',#12198,0.7);
#4681=CIRCLE('',#12199,0.5);
#4682=CIRCLE('',#12202,0.5);
#4683=CIRCLE('',#12204,0.4);
#4684=CIRCLE('',#12205,0.4);
#4685=CIRCLE('',#12208,0.5);
#4686=CIRCLE('',#12213,0.505);
#4687=CIRCLE('',#12214,0.505);
#4688=CIRCLE('',#12216,0.405);
#4689=CIRCLE('',#12218,0.405);
#4690=CIRCLE('',#12220,0.7);
#4691=CIRCLE('',#12221,0.7);
#4692=CIRCLE('',#12226,0.505);
#4693=CIRCLE('',#12227,0.505);
#4694=CIRCLE('',#12229,0.7);
#4695=CIRCLE('',#12230,0.7);
#4696=CIRCLE('',#12235,0.15);
#4697=CIRCLE('',#12236,0.15);
#4698=CIRCLE('',#12241,0.15);
#4699=CIRCLE('',#12242,0.15);
#4700=CIRCLE('',#12247,0.225);
#4701=CIRCLE('',#12248,0.225);
#4702=CIRCLE('',#12250,0.6);
#4703=CIRCLE('',#12251,0.6);
#4704=CIRCLE('',#12257,0.164999999999999);
#4705=CIRCLE('',#12258,0.164999999999999);
#4706=CIRCLE('',#12261,0.700000000000003);
#4707=CIRCLE('',#12262,0.5);
#4708=CIRCLE('',#12264,0.700000000000003);
#4709=CIRCLE('',#12265,0.5);
#4710=CIRCLE('',#12268,0.5);
#4711=CIRCLE('',#12270,0.399999999999999);
#4712=CIRCLE('',#12271,0.399999999999999);
#4713=CIRCLE('',#12274,0.5);
#4714=CIRCLE('',#12279,0.505000000000003);
#4715=CIRCLE('',#12280,0.505000000000003);
#4716=CIRCLE('',#12282,0.405000000000001);
#4717=CIRCLE('',#12284,0.405000000000001);
#4718=CIRCLE('',#12286,0.700000000000003);
#4719=CIRCLE('',#12287,0.700000000000003);
#4720=CIRCLE('',#12292,0.505000000000003);
#4721=CIRCLE('',#12293,0.505000000000003);
#4722=CIRCLE('',#12295,0.700000000000003);
#4723=CIRCLE('',#12296,0.700000000000003);
#4724=CIRCLE('',#12301,0.149999999999999);
#4725=CIRCLE('',#12302,0.149999999999999);
#4726=CIRCLE('',#12307,0.149999999999999);
#4727=CIRCLE('',#12308,0.149999999999999);
#4728=CIRCLE('',#12313,0.225000000000001);
#4729=CIRCLE('',#12314,0.225000000000001);
#4730=CIRCLE('',#12316,0.600000000000001);
#4731=CIRCLE('',#12317,0.600000000000001);
#4732=CIRCLE('',#12324,0.65);
#4733=CIRCLE('',#12325,0.65);
#4734=CIRCLE('',#12329,0.4);
#4735=CIRCLE('',#12330,0.4);
#4736=CIRCLE('',#12333,0.8);
#4737=CIRCLE('',#12334,0.0555);
#4738=CIRCLE('',#12335,0.611219772367581);
#4739=CIRCLE('',#12336,0.0555);
#4740=CIRCLE('',#12337,0.611219772367581);
#4741=CIRCLE('',#12338,0.0555);
#4742=CIRCLE('',#12339,0.611219772367581);
#4743=CIRCLE('',#12340,0.0555);
#4744=CIRCLE('',#12341,0.611219772367581);
#4745=CIRCLE('',#12342,0.0555);
#4746=CIRCLE('',#12343,0.611219772367581);
#4747=CIRCLE('',#12344,0.0555);
#4748=CIRCLE('',#12345,0.611219772367581);
#4749=CIRCLE('',#12346,0.0555);
#4750=CIRCLE('',#12347,0.611219772367581);
#4751=CIRCLE('',#12348,0.0555);
#4752=CIRCLE('',#12349,0.611219772367581);
#4753=CIRCLE('',#12350,0.0555);
#4754=CIRCLE('',#12351,0.611219772367581);
#4755=CIRCLE('',#12352,0.0555);
#4756=CIRCLE('',#12353,0.611219772367581);
#4757=CIRCLE('',#12354,0.0555);
#4758=CIRCLE('',#12355,0.611219772367581);
#4759=CIRCLE('',#12356,0.0555);
#4760=CIRCLE('',#12357,0.611219772367581);
#4761=CIRCLE('',#12358,0.0555);
#4762=CIRCLE('',#12359,0.611219772367581);
#4763=CIRCLE('',#12360,0.0555);
#4764=CIRCLE('',#12361,0.611219772367581);
#4765=CIRCLE('',#12362,0.0555);
#4766=CIRCLE('',#12363,0.611219772367581);
#4767=CIRCLE('',#12364,0.0555);
#4768=CIRCLE('',#12365,0.611219772367581);
#4769=CIRCLE('',#12366,0.0555);
#4770=CIRCLE('',#12367,0.611219772367581);
#4771=CIRCLE('',#12368,0.0555);
#4772=CIRCLE('',#12369,0.611219772367581);
#4773=CIRCLE('',#12370,0.0555);
#4774=CIRCLE('',#12371,0.611219772367581);
#4775=CIRCLE('',#12372,0.0555);
#4776=CIRCLE('',#12373,0.611219772367581);
#4777=CIRCLE('',#12375,0.8);
#4778=CIRCLE('',#12378,0.8);
#4779=CIRCLE('',#12379,0.0555);
#4780=CIRCLE('',#12380,0.611219772367581);
#4781=CIRCLE('',#12381,0.0555);
#4782=CIRCLE('',#12382,0.611219772367581);
#4783=CIRCLE('',#12383,0.0555);
#4784=CIRCLE('',#12384,0.611219772367581);
#4785=CIRCLE('',#12385,0.0555);
#4786=CIRCLE('',#12386,0.611219772367581);
#4787=CIRCLE('',#12387,0.0555);
#4788=CIRCLE('',#12388,0.611219772367581);
#4789=CIRCLE('',#12389,0.0555);
#4790=CIRCLE('',#12390,0.611219772367581);
#4791=CIRCLE('',#12391,0.0555);
#4792=CIRCLE('',#12392,0.611219772367581);
#4793=CIRCLE('',#12393,0.0555);
#4794=CIRCLE('',#12394,0.611219772367581);
#4795=CIRCLE('',#12395,0.0555);
#4796=CIRCLE('',#12396,0.611219772367581);
#4797=CIRCLE('',#12397,0.0555);
#4798=CIRCLE('',#12398,0.611219772367581);
#4799=CIRCLE('',#12399,0.0555);
#4800=CIRCLE('',#12400,0.611219772367581);
#4801=CIRCLE('',#12401,0.0555);
#4802=CIRCLE('',#12402,0.611219772367581);
#4803=CIRCLE('',#12403,0.0555);
#4804=CIRCLE('',#12404,0.611219772367581);
#4805=CIRCLE('',#12405,0.0555);
#4806=CIRCLE('',#12406,0.611219772367581);
#4807=CIRCLE('',#12407,0.0555);
#4808=CIRCLE('',#12408,0.611219772367581);
#4809=CIRCLE('',#12409,0.0555);
#4810=CIRCLE('',#12410,0.611219772367581);
#4811=CIRCLE('',#12411,0.0555);
#4812=CIRCLE('',#12412,0.611219772367581);
#4813=CIRCLE('',#12413,0.0555);
#4814=CIRCLE('',#12414,0.611219772367581);
#4815=CIRCLE('',#12415,0.0555);
#4816=CIRCLE('',#12416,0.611219772367581);
#4817=CIRCLE('',#12417,0.0555);
#4818=CIRCLE('',#12418,0.611219772367581);
#4819=CIRCLE('',#12420,0.8);
#4820=CIRCLE('',#12465,0.4);
#4821=CIRCLE('',#12466,0.4);
#4822=CIRCLE('',#12468,0.225);
#4823=CIRCLE('',#12470,0.399999999999999);
#4824=CIRCLE('',#12471,0.399999999999999);
#4825=CIRCLE('',#12473,0.225000000000001);
#4826=CIRCLE('',#12475,0.225);
#4827=CIRCLE('',#12477,0.225000000000001);
#4828=CIRCLE('',#12479,0.274999999999999);
#4829=CIRCLE('',#12480,0.274999999999999);
#4830=CIRCLE('',#12482,0.275);
#4831=CIRCLE('',#12483,0.275);
#4832=CIRCLE('',#12485,0.275);
#4833=CIRCLE('',#12486,0.275);
#4834=CIRCLE('',#12488,0.274999999999999);
#4835=CIRCLE('',#12489,0.274999999999999);
#4836=CIRCLE('',#12498,0.164999999999999);
#4837=CIRCLE('',#12499,0.164999999999999);
#4838=CIRCLE('',#12502,0.164999999999999);
#4839=CIRCLE('',#12503,0.164999999999999);
#4840=CIRCLE('',#12506,0.6);
#4841=CIRCLE('',#12508,0.6);
#4842=CIRCLE('',#12510,0.600000000000001);
#4843=CIRCLE('',#12511,0.600000000000001);
#4844=CIRCLE('',#12516,0.164999999999999);
#4845=CIRCLE('',#12517,0.164999999999999);
#4846=CIRCLE('',#12520,0.164999999999999);
#4847=CIRCLE('',#12521,0.164999999999999);
#4848=CIRCLE('',#12539,0.21);
#4849=CIRCLE('',#12541,0.21);
#4850=CIRCLE('',#12542,0.21);
#4851=CIRCLE('',#12543,0.21);
#4852=CIRCLE('',#12545,0.21);
#4853=CIRCLE('',#12547,0.21);
#4854=CIRCLE('',#12548,0.21);
#4855=CIRCLE('',#12549,0.21);
#4856=CIRCLE('',#12551,0.21);
#4857=CIRCLE('',#12553,0.21);
#4858=CIRCLE('',#12554,0.21);
#4859=CIRCLE('',#12555,0.21);
#4860=CIRCLE('',#12557,0.21);
#4861=CIRCLE('',#12559,0.21);
#4862=CIRCLE('',#12560,0.21);
#4863=CIRCLE('',#12561,0.21);
#4864=CIRCLE('',#12603,0.285);
#4865=CIRCLE('',#12604,0.265);
#4866=CIRCLE('',#12606,0.265);
#4867=CIRCLE('',#12608,0.5);
#4868=CIRCLE('',#12610,0.5);
#4869=CIRCLE('',#12614,0.375);
#4870=CIRCLE('',#12616,0.425);
#4871=CIRCLE('',#12618,0.425);
#4872=CIRCLE('',#12620,0.395);
#4873=CIRCLE('',#12622,0.27);
#4874=CIRCLE('',#12624,0.24505);
#4875=CIRCLE('',#12626,0.24505);
#4876=CIRCLE('',#12628,0.2);
#4877=CIRCLE('',#12648,0.1954);
#4878=CIRCLE('',#12650,0.3);
#4879=CIRCLE('',#12652,0.35);
#4880=CIRCLE('',#12654,0.35);
#4881=CIRCLE('',#12656,0.32);
#4882=CIRCLE('',#12658,0.22);
#4883=CIRCLE('',#12660,0.1954);
#4884=CIRCLE('',#12664,0.3);
#4885=CIRCLE('',#12666,0.35);
#4886=CIRCLE('',#12668,0.35);
#4887=CIRCLE('',#12670,0.32);
#4888=CIRCLE('',#12672,0.22);
#4889=CIRCLE('',#12674,0.1954);
#4890=CIRCLE('',#12676,0.1954);
#4891=CIRCLE('',#12678,0.16);
#4892=VERTEX_POINT('',#16236);
#4893=VERTEX_POINT('',#16238);
#4894=VERTEX_POINT('',#16243);
#4895=VERTEX_POINT('',#16245);
#4896=VERTEX_POINT('',#16250);
#4897=VERTEX_POINT('',#16252);
#4898=VERTEX_POINT('',#16257);
#4899=VERTEX_POINT('',#16259);
#4900=VERTEX_POINT('',#16264);
#4901=VERTEX_POINT('',#16266);
#4902=VERTEX_POINT('',#16271);
#4903=VERTEX_POINT('',#16273);
#4904=VERTEX_POINT('',#16278);
#4905=VERTEX_POINT('',#16280);
#4906=VERTEX_POINT('',#16285);
#4907=VERTEX_POINT('',#16287);
#4908=VERTEX_POINT('',#16292);
#4909=VERTEX_POINT('',#16294);
#4910=VERTEX_POINT('',#16298);
#4911=VERTEX_POINT('',#16300);
#4912=VERTEX_POINT('',#16304);
#4913=VERTEX_POINT('',#16306);
#4914=VERTEX_POINT('',#16310);
#4915=VERTEX_POINT('',#16312);
#4916=VERTEX_POINT('',#16316);
#4917=VERTEX_POINT('',#16318);
#4918=VERTEX_POINT('',#16323);
#4919=VERTEX_POINT('',#16325);
#4920=VERTEX_POINT('',#16330);
#4921=VERTEX_POINT('',#16332);
#4922=VERTEX_POINT('',#16337);
#4923=VERTEX_POINT('',#16339);
#4924=VERTEX_POINT('',#16344);
#4925=VERTEX_POINT('',#16346);
#4926=VERTEX_POINT('',#16351);
#4927=VERTEX_POINT('',#16353);
#4928=VERTEX_POINT('',#16358);
#4929=VERTEX_POINT('',#16360);
#4930=VERTEX_POINT('',#16365);
#4931=VERTEX_POINT('',#16367);
#4932=VERTEX_POINT('',#16372);
#4933=VERTEX_POINT('',#16373);
#4934=VERTEX_POINT('',#16375);
#4935=VERTEX_POINT('',#16377);
#4936=VERTEX_POINT('',#16381);
#4937=VERTEX_POINT('',#16383);
#4938=VERTEX_POINT('',#16387);
#4939=VERTEX_POINT('',#16389);
#4940=VERTEX_POINT('',#16399);
#4941=VERTEX_POINT('',#16400);
#4942=VERTEX_POINT('',#16402);
#4943=VERTEX_POINT('',#16404);
#4944=VERTEX_POINT('',#16408);
#4945=VERTEX_POINT('',#16410);
#4946=VERTEX_POINT('',#16414);
#4947=VERTEX_POINT('',#16418);
#4948=VERTEX_POINT('',#16425);
#4949=VERTEX_POINT('',#16426);
#4950=VERTEX_POINT('',#16428);
#4951=VERTEX_POINT('',#16430);
#4952=VERTEX_POINT('',#16434);
#4953=VERTEX_POINT('',#16435);
#4954=VERTEX_POINT('',#16440);
#4955=VERTEX_POINT('',#16444);
#4956=VERTEX_POINT('',#16452);
#4957=VERTEX_POINT('',#16453);
#4958=VERTEX_POINT('',#16455);
#4959=VERTEX_POINT('',#16457);
#4960=VERTEX_POINT('',#16461);
#4961=VERTEX_POINT('',#16463);
#4962=VERTEX_POINT('',#16467);
#4963=VERTEX_POINT('',#16471);
#4964=VERTEX_POINT('',#16478);
#4965=VERTEX_POINT('',#16479);
#4966=VERTEX_POINT('',#16481);
#4967=VERTEX_POINT('',#16483);
#4968=VERTEX_POINT('',#16487);
#4969=VERTEX_POINT('',#16488);
#4970=VERTEX_POINT('',#16493);
#4971=VERTEX_POINT('',#16497);
#4972=VERTEX_POINT('',#16505);
#4973=VERTEX_POINT('',#16507);
#4974=VERTEX_POINT('',#16511);
#4975=VERTEX_POINT('',#16513);
#4976=VERTEX_POINT('',#16517);
#4977=VERTEX_POINT('',#16519);
#4978=VERTEX_POINT('',#16523);
#4979=VERTEX_POINT('',#16525);
#4980=VERTEX_POINT('',#16529);
#4981=VERTEX_POINT('',#16531);
#4982=VERTEX_POINT('',#16535);
#4983=VERTEX_POINT('',#16537);
#4984=VERTEX_POINT('',#16541);
#4985=VERTEX_POINT('',#16543);
#4986=VERTEX_POINT('',#16547);
#4987=VERTEX_POINT('',#16549);
#4988=VERTEX_POINT('',#16553);
#4989=VERTEX_POINT('',#16555);
#4990=VERTEX_POINT('',#16559);
#4991=VERTEX_POINT('',#16560);
#4992=VERTEX_POINT('',#16562);
#4993=VERTEX_POINT('',#16564);
#4994=VERTEX_POINT('',#16568);
#4995=VERTEX_POINT('',#16569);
#4996=VERTEX_POINT('',#16571);
#4997=VERTEX_POINT('',#16573);
#4998=VERTEX_POINT('',#16577);
#4999=VERTEX_POINT('',#16579);
#5000=VERTEX_POINT('',#16583);
#5001=VERTEX_POINT('',#16585);
#5002=VERTEX_POINT('',#16589);
#5003=VERTEX_POINT('',#16591);
#5004=VERTEX_POINT('',#16596);
#5005=VERTEX_POINT('',#16600);
#5006=VERTEX_POINT('',#16610);
#5007=VERTEX_POINT('',#16612);
#5008=VERTEX_POINT('',#16616);
#5009=VERTEX_POINT('',#16618);
#5010=VERTEX_POINT('',#16625);
#5011=VERTEX_POINT('',#16626);
#5012=VERTEX_POINT('',#16628);
#5013=VERTEX_POINT('',#16630);
#5014=VERTEX_POINT('',#16634);
#5015=VERTEX_POINT('',#16635);
#5016=VERTEX_POINT('',#16637);
#5017=VERTEX_POINT('',#16639);
#5018=VERTEX_POINT('',#16643);
#5019=VERTEX_POINT('',#16644);
#5020=VERTEX_POINT('',#16646);
#5021=VERTEX_POINT('',#16648);
#5022=VERTEX_POINT('',#16652);
#5023=VERTEX_POINT('',#16653);
#5024=VERTEX_POINT('',#16655);
#5025=VERTEX_POINT('',#16657);
#5026=VERTEX_POINT('',#16665);
#5027=VERTEX_POINT('',#16676);
#5028=VERTEX_POINT('',#16678);
#5029=VERTEX_POINT('',#16682);
#5030=VERTEX_POINT('',#16689);
#5031=VERTEX_POINT('',#16690);
#5032=VERTEX_POINT('',#16692);
#5033=VERTEX_POINT('',#16694);
#5034=VERTEX_POINT('',#16698);
#5035=VERTEX_POINT('',#16699);
#5036=VERTEX_POINT('',#16701);
#5037=VERTEX_POINT('',#16703);
#5038=VERTEX_POINT('',#16707);
#5039=VERTEX_POINT('',#16708);
#5040=VERTEX_POINT('',#16710);
#5041=VERTEX_POINT('',#16712);
#5042=VERTEX_POINT('',#16716);
#5043=VERTEX_POINT('',#16717);
#5044=VERTEX_POINT('',#16719);
#5045=VERTEX_POINT('',#16721);
#5046=VERTEX_POINT('',#16729);
#5047=VERTEX_POINT('',#16740);
#5048=VERTEX_POINT('',#16744);
#5049=VERTEX_POINT('',#16747);
#5050=VERTEX_POINT('',#16753);
#5051=VERTEX_POINT('',#16755);
#5052=VERTEX_POINT('',#16759);
#5053=VERTEX_POINT('',#16761);
#5054=VERTEX_POINT('',#16765);
#5055=VERTEX_POINT('',#16767);
#5056=VERTEX_POINT('',#16771);
#5057=VERTEX_POINT('',#16773);
#5058=VERTEX_POINT('',#16777);
#5059=VERTEX_POINT('',#16779);
#5060=VERTEX_POINT('',#16783);
#5061=VERTEX_POINT('',#16785);
#5062=VERTEX_POINT('',#16789);
#5063=VERTEX_POINT('',#16791);
#5064=VERTEX_POINT('',#16795);
#5065=VERTEX_POINT('',#16797);
#5066=VERTEX_POINT('',#16801);
#5067=VERTEX_POINT('',#16803);
#5068=VERTEX_POINT('',#16807);
#5069=VERTEX_POINT('',#16808);
#5070=VERTEX_POINT('',#16810);
#5071=VERTEX_POINT('',#16812);
#5072=VERTEX_POINT('',#16816);
#5073=VERTEX_POINT('',#16817);
#5074=VERTEX_POINT('',#16819);
#5075=VERTEX_POINT('',#16821);
#5076=VERTEX_POINT('',#16825);
#5077=VERTEX_POINT('',#16827);
#5078=VERTEX_POINT('',#16831);
#5079=VERTEX_POINT('',#16833);
#5080=VERTEX_POINT('',#16837);
#5081=VERTEX_POINT('',#16839);
#5082=VERTEX_POINT('',#16844);
#5083=VERTEX_POINT('',#16848);
#5084=VERTEX_POINT('',#16858);
#5085=VERTEX_POINT('',#16860);
#5086=VERTEX_POINT('',#16864);
#5087=VERTEX_POINT('',#16866);
#5088=VERTEX_POINT('',#16873);
#5089=VERTEX_POINT('',#16874);
#5090=VERTEX_POINT('',#16876);
#5091=VERTEX_POINT('',#16878);
#5092=VERTEX_POINT('',#16882);
#5093=VERTEX_POINT('',#16883);
#5094=VERTEX_POINT('',#16885);
#5095=VERTEX_POINT('',#16887);
#5096=VERTEX_POINT('',#16891);
#5097=VERTEX_POINT('',#16892);
#5098=VERTEX_POINT('',#16894);
#5099=VERTEX_POINT('',#16896);
#5100=VERTEX_POINT('',#16900);
#5101=VERTEX_POINT('',#16901);
#5102=VERTEX_POINT('',#16903);
#5103=VERTEX_POINT('',#16905);
#5104=VERTEX_POINT('',#16913);
#5105=VERTEX_POINT('',#16924);
#5106=VERTEX_POINT('',#16926);
#5107=VERTEX_POINT('',#16930);
#5108=VERTEX_POINT('',#16937);
#5109=VERTEX_POINT('',#16938);
#5110=VERTEX_POINT('',#16940);
#5111=VERTEX_POINT('',#16942);
#5112=VERTEX_POINT('',#16946);
#5113=VERTEX_POINT('',#16947);
#5114=VERTEX_POINT('',#16949);
#5115=VERTEX_POINT('',#16951);
#5116=VERTEX_POINT('',#16955);
#5117=VERTEX_POINT('',#16956);
#5118=VERTEX_POINT('',#16958);
#5119=VERTEX_POINT('',#16960);
#5120=VERTEX_POINT('',#16964);
#5121=VERTEX_POINT('',#16965);
#5122=VERTEX_POINT('',#16967);
#5123=VERTEX_POINT('',#16969);
#5124=VERTEX_POINT('',#16977);
#5125=VERTEX_POINT('',#16988);
#5126=VERTEX_POINT('',#16992);
#5127=VERTEX_POINT('',#16995);
#5128=VERTEX_POINT('',#17001);
#5129=VERTEX_POINT('',#17002);
#5130=VERTEX_POINT('',#17004);
#5131=VERTEX_POINT('',#17006);
#5132=VERTEX_POINT('',#17010);
#5133=VERTEX_POINT('',#17011);
#5134=VERTEX_POINT('',#17013);
#5135=VERTEX_POINT('',#17015);
#5136=VERTEX_POINT('',#17019);
#5137=VERTEX_POINT('',#17020);
#5138=VERTEX_POINT('',#17022);
#5139=VERTEX_POINT('',#17024);
#5140=VERTEX_POINT('',#17034);
#5141=VERTEX_POINT('',#17036);
#5142=VERTEX_POINT('',#17040);
#5143=VERTEX_POINT('',#17044);
#5144=VERTEX_POINT('',#17052);
#5145=VERTEX_POINT('',#17053);
#5146=VERTEX_POINT('',#17055);
#5147=VERTEX_POINT('',#17057);
#5148=VERTEX_POINT('',#17061);
#5149=VERTEX_POINT('',#17062);
#5150=VERTEX_POINT('',#17064);
#5151=VERTEX_POINT('',#17066);
#5152=VERTEX_POINT('',#17072);
#5153=VERTEX_POINT('',#17075);
#5154=VERTEX_POINT('',#17076);
#5155=VERTEX_POINT('',#17078);
#5156=VERTEX_POINT('',#17080);
#5157=VERTEX_POINT('',#17084);
#5158=VERTEX_POINT('',#17085);
#5159=VERTEX_POINT('',#17087);
#5160=VERTEX_POINT('',#17089);
#5161=VERTEX_POINT('',#17095);
#5162=VERTEX_POINT('',#17098);
#5163=VERTEX_POINT('',#17100);
#5164=VERTEX_POINT('',#17102);
#5165=VERTEX_POINT('',#17104);
#5166=VERTEX_POINT('',#17106);
#5167=VERTEX_POINT('',#17108);
#5168=VERTEX_POINT('',#17110);
#5169=VERTEX_POINT('',#17112);
#5170=VERTEX_POINT('',#17117);
#5171=VERTEX_POINT('',#17121);
#5172=VERTEX_POINT('',#17127);
#5173=VERTEX_POINT('',#17131);
#5174=VERTEX_POINT('',#17135);
#5175=VERTEX_POINT('',#17137);
#5176=VERTEX_POINT('',#17141);
#5177=VERTEX_POINT('',#17143);
#5178=VERTEX_POINT('',#17149);
#5179=VERTEX_POINT('',#17152);
#5180=VERTEX_POINT('',#17163);
#5181=VERTEX_POINT('',#17164);
#5182=VERTEX_POINT('',#17166);
#5183=VERTEX_POINT('',#17168);
#5184=VERTEX_POINT('',#17172);
#5185=VERTEX_POINT('',#17173);
#5186=VERTEX_POINT('',#17175);
#5187=VERTEX_POINT('',#17177);
#5188=VERTEX_POINT('',#17183);
#5189=VERTEX_POINT('',#17186);
#5190=VERTEX_POINT('',#17187);
#5191=VERTEX_POINT('',#17189);
#5192=VERTEX_POINT('',#17191);
#5193=VERTEX_POINT('',#17195);
#5194=VERTEX_POINT('',#17196);
#5195=VERTEX_POINT('',#17198);
#5196=VERTEX_POINT('',#17200);
#5197=VERTEX_POINT('',#17206);
#5198=VERTEX_POINT('',#17209);
#5199=VERTEX_POINT('',#17211);
#5200=VERTEX_POINT('',#17213);
#5201=VERTEX_POINT('',#17215);
#5202=VERTEX_POINT('',#17217);
#5203=VERTEX_POINT('',#17219);
#5204=VERTEX_POINT('',#17221);
#5205=VERTEX_POINT('',#17223);
#5206=VERTEX_POINT('',#17228);
#5207=VERTEX_POINT('',#17232);
#5208=VERTEX_POINT('',#17238);
#5209=VERTEX_POINT('',#17242);
#5210=VERTEX_POINT('',#17246);
#5211=VERTEX_POINT('',#17248);
#5212=VERTEX_POINT('',#17252);
#5213=VERTEX_POINT('',#17254);
#5214=VERTEX_POINT('',#17260);
#5215=VERTEX_POINT('',#17263);
#5216=VERTEX_POINT('',#17275);
#5217=VERTEX_POINT('',#17276);
#5218=VERTEX_POINT('',#17279);
#5219=VERTEX_POINT('',#17281);
#5220=VERTEX_POINT('',#17285);
#5221=VERTEX_POINT('',#17289);
#5222=VERTEX_POINT('',#17291);
#5223=VERTEX_POINT('',#17295);
#5224=VERTEX_POINT('',#17300);
#5225=VERTEX_POINT('',#17304);
#5226=VERTEX_POINT('',#17310);
#5227=VERTEX_POINT('',#17311);
#5228=VERTEX_POINT('',#17314);
#5229=VERTEX_POINT('',#17316);
#5230=VERTEX_POINT('',#17320);
#5231=VERTEX_POINT('',#17324);
#5232=VERTEX_POINT('',#17326);
#5233=VERTEX_POINT('',#17329);
#5234=VERTEX_POINT('',#17333);
#5235=VERTEX_POINT('',#17337);
#5236=VERTEX_POINT('',#17345);
#5237=VERTEX_POINT('',#17346);
#5238=VERTEX_POINT('',#17349);
#5239=VERTEX_POINT('',#17350);
#5240=VERTEX_POINT('',#17353);
#5241=VERTEX_POINT('',#17354);
#5242=VERTEX_POINT('',#17357);
#5243=VERTEX_POINT('',#17358);
#5244=VERTEX_POINT('',#17361);
#5245=VERTEX_POINT('',#17362);
#5246=VERTEX_POINT('',#17365);
#5247=VERTEX_POINT('',#17366);
#5248=VERTEX_POINT('',#17369);
#5249=VERTEX_POINT('',#17370);
#5250=VERTEX_POINT('',#17373);
#5251=VERTEX_POINT('',#17374);
#5252=VERTEX_POINT('',#17378);
#5253=VERTEX_POINT('',#17379);
#5254=VERTEX_POINT('',#17402);
#5255=VERTEX_POINT('',#17404);
#5256=VERTEX_POINT('',#17429);
#5257=VERTEX_POINT('',#17431);
#5258=VERTEX_POINT('',#17454);
#5259=VERTEX_POINT('',#17456);
#5260=VERTEX_POINT('',#17479);
#5261=VERTEX_POINT('',#17481);
#5262=VERTEX_POINT('',#17494);
#5263=VERTEX_POINT('',#17497);
#5264=VERTEX_POINT('',#17510);
#5265=VERTEX_POINT('',#17512);
#5266=VERTEX_POINT('',#17535);
#5267=VERTEX_POINT('',#17537);
#5268=VERTEX_POINT('',#17560);
#5269=VERTEX_POINT('',#17562);
#5270=VERTEX_POINT('',#17585);
#5271=VERTEX_POINT('',#17587);
#5272=VERTEX_POINT('',#17612);
#5273=VERTEX_POINT('',#17616);
#5274=VERTEX_POINT('',#17641);
#5275=VERTEX_POINT('',#17645);
#5276=VERTEX_POINT('',#17670);
#5277=VERTEX_POINT('',#17674);
#5278=VERTEX_POINT('',#17675);
#5279=VERTEX_POINT('',#17702);
#5280=VERTEX_POINT('',#17706);
#5281=VERTEX_POINT('',#17731);
#5282=VERTEX_POINT('',#17735);
#5283=VERTEX_POINT('',#17760);
#5284=VERTEX_POINT('',#17764);
#5285=VERTEX_POINT('',#17789);
#5286=VERTEX_POINT('',#17792);
#5287=VERTEX_POINT('',#17794);
#5288=VERTEX_POINT('',#17826);
#5289=VERTEX_POINT('',#17828);
#5290=VERTEX_POINT('',#17831);
#5291=VERTEX_POINT('',#17835);
#5292=VERTEX_POINT('',#17840);
#5293=VERTEX_POINT('',#17842);
#5294=VERTEX_POINT('',#17845);
#5295=VERTEX_POINT('',#17849);
#5296=VERTEX_POINT('',#17860);
#5297=VERTEX_POINT('',#17861);
#5298=VERTEX_POINT('',#17863);
#5299=VERTEX_POINT('',#17865);
#5300=VERTEX_POINT('',#17869);
#5301=VERTEX_POINT('',#17871);
#5302=VERTEX_POINT('',#17875);
#5303=VERTEX_POINT('',#17877);
#5304=VERTEX_POINT('',#17881);
#5305=VERTEX_POINT('',#17883);
#5306=VERTEX_POINT('',#17887);
#5307=VERTEX_POINT('',#17889);
#5308=VERTEX_POINT('',#17893);
#5309=VERTEX_POINT('',#17895);
#5310=VERTEX_POINT('',#17899);
#5311=VERTEX_POINT('',#17901);
#5312=VERTEX_POINT('',#17905);
#5313=VERTEX_POINT('',#17907);
#5314=VERTEX_POINT('',#17911);
#5315=VERTEX_POINT('',#17913);
#5316=VERTEX_POINT('',#17917);
#5317=VERTEX_POINT('',#17918);
#5318=VERTEX_POINT('',#17920);
#5319=VERTEX_POINT('',#17922);
#5320=VERTEX_POINT('',#17926);
#5321=VERTEX_POINT('',#17928);
#5322=VERTEX_POINT('',#17932);
#5323=VERTEX_POINT('',#17934);
#5324=VERTEX_POINT('',#17938);
#5325=VERTEX_POINT('',#17940);
#5326=VERTEX_POINT('',#17944);
#5327=VERTEX_POINT('',#17946);
#5328=VERTEX_POINT('',#17950);
#5329=VERTEX_POINT('',#17952);
#5330=VERTEX_POINT('',#17956);
#5331=VERTEX_POINT('',#17958);
#5332=VERTEX_POINT('',#17962);
#5333=VERTEX_POINT('',#17964);
#5334=VERTEX_POINT('',#17968);
#5335=VERTEX_POINT('',#17970);
#5336=VERTEX_POINT('',#17974);
#5337=VERTEX_POINT('',#17975);
#5338=VERTEX_POINT('',#17977);
#5339=VERTEX_POINT('',#17979);
#5340=VERTEX_POINT('',#17983);
#5341=VERTEX_POINT('',#17985);
#5342=VERTEX_POINT('',#17989);
#5343=VERTEX_POINT('',#17991);
#5344=VERTEX_POINT('',#17995);
#5345=VERTEX_POINT('',#17997);
#5346=VERTEX_POINT('',#18001);
#5347=VERTEX_POINT('',#18003);
#5348=VERTEX_POINT('',#18007);
#5349=VERTEX_POINT('',#18009);
#5350=VERTEX_POINT('',#18013);
#5351=VERTEX_POINT('',#18015);
#5352=VERTEX_POINT('',#18019);
#5353=VERTEX_POINT('',#18021);
#5354=VERTEX_POINT('',#18025);
#5355=VERTEX_POINT('',#18027);
#5356=VERTEX_POINT('',#18031);
#5357=VERTEX_POINT('',#18032);
#5358=VERTEX_POINT('',#18034);
#5359=VERTEX_POINT('',#18036);
#5360=VERTEX_POINT('',#18040);
#5361=VERTEX_POINT('',#18042);
#5362=VERTEX_POINT('',#18046);
#5363=VERTEX_POINT('',#18048);
#5364=VERTEX_POINT('',#18052);
#5365=VERTEX_POINT('',#18054);
#5366=VERTEX_POINT('',#18058);
#5367=VERTEX_POINT('',#18060);
#5368=VERTEX_POINT('',#18064);
#5369=VERTEX_POINT('',#18066);
#5370=VERTEX_POINT('',#18070);
#5371=VERTEX_POINT('',#18072);
#5372=VERTEX_POINT('',#18076);
#5373=VERTEX_POINT('',#18078);
#5374=VERTEX_POINT('',#18082);
#5375=VERTEX_POINT('',#18084);
#5376=VERTEX_POINT('',#18088);
#5377=VERTEX_POINT('',#18090);
#5378=VERTEX_POINT('',#18094);
#5379=VERTEX_POINT('',#18096);
#5380=VERTEX_POINT('',#18100);
#5381=VERTEX_POINT('',#18102);
#5382=VERTEX_POINT('',#18109);
#5383=VERTEX_POINT('',#18111);
#5384=VERTEX_POINT('',#18118);
#5385=VERTEX_POINT('',#18120);
#5386=VERTEX_POINT('',#18133);
#5387=VERTEX_POINT('',#18134);
#5388=VERTEX_POINT('',#18136);
#5389=VERTEX_POINT('',#18138);
#5390=VERTEX_POINT('',#18142);
#5391=VERTEX_POINT('',#18144);
#5392=VERTEX_POINT('',#18148);
#5393=VERTEX_POINT('',#18150);
#5394=VERTEX_POINT('',#18153);
#5395=VERTEX_POINT('',#18156);
#5396=VERTEX_POINT('',#18158);
#5397=VERTEX_POINT('',#18160);
#5398=VERTEX_POINT('',#18162);
#5399=VERTEX_POINT('',#18164);
#5400=VERTEX_POINT('',#18166);
#5401=VERTEX_POINT('',#18170);
#5402=VERTEX_POINT('',#18174);
#5403=VERTEX_POINT('',#18178);
#5404=VERTEX_POINT('',#18180);
#5405=VERTEX_POINT('',#18182);
#5406=VERTEX_POINT('',#18184);
#5407=VERTEX_POINT('',#18190);
#5408=VERTEX_POINT('',#18192);
#5409=VERTEX_POINT('',#18196);
#5410=VERTEX_POINT('',#18199);
#5411=VERTEX_POINT('',#18201);
#5412=VERTEX_POINT('',#18213);
#5413=VERTEX_POINT('',#18214);
#5414=VERTEX_POINT('',#18216);
#5415=VERTEX_POINT('',#18218);
#5416=VERTEX_POINT('',#18222);
#5417=VERTEX_POINT('',#18224);
#5418=VERTEX_POINT('',#18228);
#5419=VERTEX_POINT('',#18230);
#5420=VERTEX_POINT('',#18234);
#5421=VERTEX_POINT('',#18236);
#5422=VERTEX_POINT('',#18240);
#5423=VERTEX_POINT('',#18242);
#5424=VERTEX_POINT('',#18251);
#5425=VERTEX_POINT('',#18254);
#5426=VERTEX_POINT('',#18257);
#5427=VERTEX_POINT('',#18261);
#5428=VERTEX_POINT('',#18265);
#5429=VERTEX_POINT('',#18269);
#5430=VERTEX_POINT('',#18272);
#5431=VERTEX_POINT('',#18279);
#5432=VERTEX_POINT('',#18281);
#5433=VERTEX_POINT('',#18285);
#5434=VERTEX_POINT('',#18288);
#5435=VERTEX_POINT('',#18290);
#5436=VERTEX_POINT('',#18294);
#5437=VERTEX_POINT('',#18297);
#5438=VERTEX_POINT('',#18299);
#5439=VERTEX_POINT('',#18303);
#5440=VERTEX_POINT('',#18306);
#5441=VERTEX_POINT('',#18308);
#5442=VERTEX_POINT('',#18312);
#5443=VERTEX_POINT('',#18315);
#5444=VERTEX_POINT('',#18319);
#5445=VERTEX_POINT('',#18323);
#5446=VERTEX_POINT('',#18327);
#5447=VERTEX_POINT('',#18331);
#5448=VERTEX_POINT('',#18332);
#5449=VERTEX_POINT('',#18334);
#5450=VERTEX_POINT('',#18336);
#5451=VERTEX_POINT('',#18340);
#5452=VERTEX_POINT('',#18342);
#5453=VERTEX_POINT('',#18346);
#5454=VERTEX_POINT('',#18348);
#5455=VERTEX_POINT('',#18352);
#5456=VERTEX_POINT('',#18354);
#5457=VERTEX_POINT('',#18358);
#5458=VERTEX_POINT('',#18360);
#5459=VERTEX_POINT('',#18364);
#5460=VERTEX_POINT('',#18366);
#5461=VERTEX_POINT('',#18370);
#5462=VERTEX_POINT('',#18372);
#5463=VERTEX_POINT('',#18376);
#5464=VERTEX_POINT('',#18378);
#5465=VERTEX_POINT('',#18382);
#5466=VERTEX_POINT('',#18384);
#5467=VERTEX_POINT('',#18388);
#5468=VERTEX_POINT('',#18390);
#5469=VERTEX_POINT('',#18394);
#5470=VERTEX_POINT('',#18396);
#5471=VERTEX_POINT('',#18407);
#5472=VERTEX_POINT('',#18409);
#5473=VERTEX_POINT('',#18414);
#5474=VERTEX_POINT('',#18416);
#5475=VERTEX_POINT('',#18419);
#5476=VERTEX_POINT('',#18421);
#5477=VERTEX_POINT('',#18426);
#5478=VERTEX_POINT('',#18430);
#5479=VERTEX_POINT('',#18432);
#5480=VERTEX_POINT('',#18437);
#5481=VERTEX_POINT('',#18444);
#5482=VERTEX_POINT('',#18446);
#5483=VERTEX_POINT('',#18450);
#5484=VERTEX_POINT('',#18453);
#5485=VERTEX_POINT('',#18457);
#5486=VERTEX_POINT('',#18459);
#5487=VERTEX_POINT('',#18466);
#5488=VERTEX_POINT('',#18468);
#5489=VERTEX_POINT('',#18472);
#5490=VERTEX_POINT('',#18474);
#5491=VERTEX_POINT('',#18481);
#5492=VERTEX_POINT('',#18483);
#5493=VERTEX_POINT('',#18490);
#5494=VERTEX_POINT('',#18492);
#5495=VERTEX_POINT('',#18499);
#5496=VERTEX_POINT('',#18501);
#5497=VERTEX_POINT('',#18505);
#5498=VERTEX_POINT('',#18507);
#5499=VERTEX_POINT('',#18515);
#5500=VERTEX_POINT('',#18517);
#5501=VERTEX_POINT('',#18522);
#5502=VERTEX_POINT('',#18524);
#5503=VERTEX_POINT('',#18527);
#5504=VERTEX_POINT('',#18529);
#5505=VERTEX_POINT('',#18534);
#5506=VERTEX_POINT('',#18538);
#5507=VERTEX_POINT('',#18540);
#5508=VERTEX_POINT('',#18545);
#5509=VERTEX_POINT('',#18552);
#5510=VERTEX_POINT('',#18554);
#5511=VERTEX_POINT('',#18558);
#5512=VERTEX_POINT('',#18561);
#5513=VERTEX_POINT('',#18565);
#5514=VERTEX_POINT('',#18567);
#5515=VERTEX_POINT('',#18574);
#5516=VERTEX_POINT('',#18576);
#5517=VERTEX_POINT('',#18580);
#5518=VERTEX_POINT('',#18582);
#5519=VERTEX_POINT('',#18589);
#5520=VERTEX_POINT('',#18591);
#5521=VERTEX_POINT('',#18598);
#5522=VERTEX_POINT('',#18600);
#5523=VERTEX_POINT('',#18607);
#5524=VERTEX_POINT('',#18609);
#5525=VERTEX_POINT('',#18613);
#5526=VERTEX_POINT('',#18615);
#5527=VERTEX_POINT('',#18622);
#5528=VERTEX_POINT('',#18623);
#5529=VERTEX_POINT('',#18634);
#5530=VERTEX_POINT('',#18663);
#5531=VERTEX_POINT('',#18665);
#5532=VERTEX_POINT('',#18676);
#5533=VERTEX_POINT('',#18687);
#5534=VERTEX_POINT('',#18709);
#5535=VERTEX_POINT('',#18710);
#5536=VERTEX_POINT('',#18747);
#5537=VERTEX_POINT('',#18749);
#5538=VERTEX_POINT('',#18760);
#5539=VERTEX_POINT('',#18790);
#5540=VERTEX_POINT('',#18793);
#5541=VERTEX_POINT('',#18796);
#5542=VERTEX_POINT('',#18797);
#5543=VERTEX_POINT('',#18816);
#5544=VERTEX_POINT('',#18837);
#5545=VERTEX_POINT('',#18838);
#5546=VERTEX_POINT('',#18857);
#5547=VERTEX_POINT('',#18879);
#5548=VERTEX_POINT('',#18881);
#5549=VERTEX_POINT('',#18919);
#5550=VERTEX_POINT('',#18920);
#5551=VERTEX_POINT('',#18959);
#5552=VERTEX_POINT('',#18962);
#5553=VERTEX_POINT('',#18967);
#5554=VERTEX_POINT('',#18969);
#5555=VERTEX_POINT('',#18970);
#5556=VERTEX_POINT('',#18972);
#5557=VERTEX_POINT('',#18974);
#5558=VERTEX_POINT('',#18976);
#5559=VERTEX_POINT('',#18978);
#5560=VERTEX_POINT('',#18980);
#5561=VERTEX_POINT('',#18982);
#5562=VERTEX_POINT('',#18984);
#5563=VERTEX_POINT('',#18986);
#5564=VERTEX_POINT('',#18988);
#5565=VERTEX_POINT('',#18990);
#5566=VERTEX_POINT('',#18992);
#5567=VERTEX_POINT('',#18994);
#5568=VERTEX_POINT('',#18996);
#5569=VERTEX_POINT('',#18998);
#5570=VERTEX_POINT('',#19000);
#5571=VERTEX_POINT('',#19002);
#5572=VERTEX_POINT('',#19004);
#5573=VERTEX_POINT('',#19006);
#5574=VERTEX_POINT('',#19008);
#5575=VERTEX_POINT('',#19010);
#5576=VERTEX_POINT('',#19012);
#5577=VERTEX_POINT('',#19014);
#5578=VERTEX_POINT('',#19016);
#5579=VERTEX_POINT('',#19018);
#5580=VERTEX_POINT('',#19020);
#5581=VERTEX_POINT('',#19022);
#5582=VERTEX_POINT('',#19024);
#5583=VERTEX_POINT('',#19026);
#5584=VERTEX_POINT('',#19028);
#5585=VERTEX_POINT('',#19030);
#5586=VERTEX_POINT('',#19032);
#5587=VERTEX_POINT('',#19034);
#5588=VERTEX_POINT('',#19036);
#5589=VERTEX_POINT('',#19038);
#5590=VERTEX_POINT('',#19040);
#5591=VERTEX_POINT('',#19042);
#5592=VERTEX_POINT('',#19044);
#5593=VERTEX_POINT('',#19046);
#5594=VERTEX_POINT('',#19050);
#5595=VERTEX_POINT('',#19055);
#5596=VERTEX_POINT('',#19057);
#5597=VERTEX_POINT('',#19058);
#5598=VERTEX_POINT('',#19060);
#5599=VERTEX_POINT('',#19062);
#5600=VERTEX_POINT('',#19064);
#5601=VERTEX_POINT('',#19066);
#5602=VERTEX_POINT('',#19068);
#5603=VERTEX_POINT('',#19070);
#5604=VERTEX_POINT('',#19072);
#5605=VERTEX_POINT('',#19074);
#5606=VERTEX_POINT('',#19076);
#5607=VERTEX_POINT('',#19078);
#5608=VERTEX_POINT('',#19080);
#5609=VERTEX_POINT('',#19082);
#5610=VERTEX_POINT('',#19084);
#5611=VERTEX_POINT('',#19086);
#5612=VERTEX_POINT('',#19088);
#5613=VERTEX_POINT('',#19090);
#5614=VERTEX_POINT('',#19092);
#5615=VERTEX_POINT('',#19094);
#5616=VERTEX_POINT('',#19096);
#5617=VERTEX_POINT('',#19098);
#5618=VERTEX_POINT('',#19100);
#5619=VERTEX_POINT('',#19102);
#5620=VERTEX_POINT('',#19104);
#5621=VERTEX_POINT('',#19106);
#5622=VERTEX_POINT('',#19108);
#5623=VERTEX_POINT('',#19110);
#5624=VERTEX_POINT('',#19112);
#5625=VERTEX_POINT('',#19114);
#5626=VERTEX_POINT('',#19116);
#5627=VERTEX_POINT('',#19118);
#5628=VERTEX_POINT('',#19120);
#5629=VERTEX_POINT('',#19122);
#5630=VERTEX_POINT('',#19124);
#5631=VERTEX_POINT('',#19126);
#5632=VERTEX_POINT('',#19128);
#5633=VERTEX_POINT('',#19130);
#5634=VERTEX_POINT('',#19132);
#5635=VERTEX_POINT('',#19134);
#5636=VERTEX_POINT('',#19138);
#5637=VERTEX_POINT('',#19225);
#5638=VERTEX_POINT('',#19227);
#5639=VERTEX_POINT('',#19231);
#5640=VERTEX_POINT('',#19234);
#5641=VERTEX_POINT('',#19236);
#5642=VERTEX_POINT('',#19240);
#5643=VERTEX_POINT('',#19243);
#5644=VERTEX_POINT('',#19247);
#5645=VERTEX_POINT('',#19251);
#5646=VERTEX_POINT('',#19253);
#5647=VERTEX_POINT('',#19257);
#5648=VERTEX_POINT('',#19259);
#5649=VERTEX_POINT('',#19263);
#5650=VERTEX_POINT('',#19265);
#5651=VERTEX_POINT('',#19269);
#5652=VERTEX_POINT('',#19271);
#5653=VERTEX_POINT('',#19275);
#5654=VERTEX_POINT('',#19276);
#5655=VERTEX_POINT('',#19278);
#5656=VERTEX_POINT('',#19280);
#5657=VERTEX_POINT('',#19284);
#5658=VERTEX_POINT('',#19286);
#5659=VERTEX_POINT('',#19290);
#5660=VERTEX_POINT('',#19292);
#5661=VERTEX_POINT('',#19302);
#5662=VERTEX_POINT('',#19304);
#5663=VERTEX_POINT('',#19309);
#5664=VERTEX_POINT('',#19311);
#5665=VERTEX_POINT('',#19316);
#5666=VERTEX_POINT('',#19317);
#5667=VERTEX_POINT('',#19319);
#5668=VERTEX_POINT('',#19321);
#5669=VERTEX_POINT('',#19325);
#5670=VERTEX_POINT('',#19327);
#5671=VERTEX_POINT('',#19331);
#5672=VERTEX_POINT('',#19332);
#5673=VERTEX_POINT('',#19334);
#5674=VERTEX_POINT('',#19336);
#5675=VERTEX_POINT('',#19340);
#5676=VERTEX_POINT('',#19342);
#5677=VERTEX_POINT('',#19346);
#5678=VERTEX_POINT('',#19348);
#5679=VERTEX_POINT('',#19350);
#5680=VERTEX_POINT('',#19352);
#5681=VERTEX_POINT('',#19357);
#5682=VERTEX_POINT('',#19361);
#5683=VERTEX_POINT('',#19363);
#5684=VERTEX_POINT('',#19368);
#5685=VERTEX_POINT('',#19370);
#5686=VERTEX_POINT('',#19375);
#5687=VERTEX_POINT('',#19377);
#5688=VERTEX_POINT('',#19381);
#5689=VERTEX_POINT('',#19393);
#5690=VERTEX_POINT('',#19394);
#5691=VERTEX_POINT('',#19396);
#5692=VERTEX_POINT('',#19398);
#5693=VERTEX_POINT('',#19402);
#5694=VERTEX_POINT('',#19404);
#5695=VERTEX_POINT('',#19408);
#5696=VERTEX_POINT('',#19410);
#5697=VERTEX_POINT('',#19421);
#5698=VERTEX_POINT('',#19422);
#5699=VERTEX_POINT('',#19426);
#5700=VERTEX_POINT('',#19428);
#5701=VERTEX_POINT('',#19430);
#5702=VERTEX_POINT('',#19433);
#5703=VERTEX_POINT('',#19437);
#5704=VERTEX_POINT('',#19438);
#5705=VERTEX_POINT('',#19442);
#5706=VERTEX_POINT('',#19444);
#5707=VERTEX_POINT('',#19446);
#5708=VERTEX_POINT('',#19449);
#5709=VERTEX_POINT('',#19453);
#5710=VERTEX_POINT('',#19454);
#5711=VERTEX_POINT('',#19458);
#5712=VERTEX_POINT('',#19460);
#5713=VERTEX_POINT('',#19462);
#5714=VERTEX_POINT('',#19465);
#5715=VERTEX_POINT('',#19469);
#5716=VERTEX_POINT('',#19470);
#5717=VERTEX_POINT('',#19474);
#5718=VERTEX_POINT('',#19476);
#5719=VERTEX_POINT('',#19478);
#5720=VERTEX_POINT('',#19481);
#5721=VERTEX_POINT('',#19486);
#5722=VERTEX_POINT('',#19488);
#5723=VERTEX_POINT('',#19490);
#5724=VERTEX_POINT('',#19492);
#5725=VERTEX_POINT('',#19497);
#5726=VERTEX_POINT('',#19499);
#5727=VERTEX_POINT('',#19501);
#5728=VERTEX_POINT('',#19503);
#5729=VERTEX_POINT('',#19507);
#5730=VERTEX_POINT('',#19509);
#5731=VERTEX_POINT('',#19511);
#5732=VERTEX_POINT('',#19513);
#5733=VERTEX_POINT('',#19516);
#5734=VERTEX_POINT('',#19518);
#5735=VERTEX_POINT('',#19520);
#5736=VERTEX_POINT('',#19522);
#5737=VERTEX_POINT('',#19526);
#5738=VERTEX_POINT('',#19530);
#5739=VERTEX_POINT('',#19534);
#5740=VERTEX_POINT('',#19538);
#5741=VERTEX_POINT('',#19544);
#5742=VERTEX_POINT('',#19548);
#5743=VERTEX_POINT('',#19552);
#5744=VERTEX_POINT('',#19556);
#5745=VERTEX_POINT('',#19564);
#5746=VERTEX_POINT('',#19565);
#5747=VERTEX_POINT('',#19567);
#5748=VERTEX_POINT('',#19569);
#5749=VERTEX_POINT('',#19573);
#5750=VERTEX_POINT('',#19575);
#5751=VERTEX_POINT('',#19579);
#5752=VERTEX_POINT('',#19581);
#5753=VERTEX_POINT('',#19585);
#5754=VERTEX_POINT('',#19587);
#5755=VERTEX_POINT('',#19591);
#5756=VERTEX_POINT('',#19593);
#5757=VERTEX_POINT('',#19597);
#5758=VERTEX_POINT('',#19599);
#5759=VERTEX_POINT('',#19603);
#5760=VERTEX_POINT('',#19605);
#5761=VERTEX_POINT('',#19615);
#5762=VERTEX_POINT('',#19616);
#5763=VERTEX_POINT('',#19618);
#5764=VERTEX_POINT('',#19620);
#5765=VERTEX_POINT('',#19624);
#5766=VERTEX_POINT('',#19626);
#5767=VERTEX_POINT('',#19630);
#5768=VERTEX_POINT('',#19632);
#5769=VERTEX_POINT('',#19636);
#5770=VERTEX_POINT('',#19638);
#5771=VERTEX_POINT('',#19642);
#5772=VERTEX_POINT('',#19644);
#5773=VERTEX_POINT('',#19648);
#5774=VERTEX_POINT('',#19650);
#5775=VERTEX_POINT('',#19654);
#5776=VERTEX_POINT('',#19656);
#5777=VERTEX_POINT('',#19669);
#5778=VERTEX_POINT('',#19671);
#5779=VERTEX_POINT('',#19675);
#5780=VERTEX_POINT('',#19679);
#5781=VERTEX_POINT('',#19682);
#5782=VERTEX_POINT('',#19688);
#5783=VERTEX_POINT('',#19691);
#5784=VERTEX_POINT('',#19695);
#5785=VERTEX_POINT('',#19699);
#5786=VERTEX_POINT('',#19703);
#5787=VERTEX_POINT('',#19706);
#5788=VERTEX_POINT('',#19710);
#5789=VERTEX_POINT('',#19714);
#5790=VERTEX_POINT('',#19719);
#5791=VERTEX_POINT('',#19720);
#5792=VERTEX_POINT('',#19722);
#5793=VERTEX_POINT('',#19724);
#5794=VERTEX_POINT('',#19728);
#5795=VERTEX_POINT('',#19730);
#5796=VERTEX_POINT('',#19734);
#5797=VERTEX_POINT('',#19736);
#5798=VERTEX_POINT('',#19740);
#5799=VERTEX_POINT('',#19742);
#5800=VERTEX_POINT('',#19746);
#5801=VERTEX_POINT('',#19748);
#5802=VERTEX_POINT('',#19758);
#5803=VERTEX_POINT('',#19759);
#5804=VERTEX_POINT('',#19761);
#5805=VERTEX_POINT('',#19763);
#5806=VERTEX_POINT('',#19767);
#5807=VERTEX_POINT('',#19769);
#5808=VERTEX_POINT('',#19773);
#5809=VERTEX_POINT('',#19775);
#5810=VERTEX_POINT('',#19779);
#5811=VERTEX_POINT('',#19781);
#5812=VERTEX_POINT('',#19785);
#5813=VERTEX_POINT('',#19787);
#5814=VERTEX_POINT('',#19796);
#5815=VERTEX_POINT('',#19799);
#5816=VERTEX_POINT('',#19802);
#5817=VERTEX_POINT('',#19806);
#5818=VERTEX_POINT('',#19810);
#5819=VERTEX_POINT('',#19814);
#5820=VERTEX_POINT('',#19817);
#5821=VERTEX_POINT('',#19824);
#5822=VERTEX_POINT('',#19827);
#5823=VERTEX_POINT('',#19831);
#5824=VERTEX_POINT('',#19835);
#5825=VERTEX_POINT('',#19839);
#5826=VERTEX_POINT('',#19842);
#5827=VERTEX_POINT('',#19846);
#5828=VERTEX_POINT('',#19850);
#5829=VERTEX_POINT('',#19855);
#5830=VERTEX_POINT('',#19856);
#5831=VERTEX_POINT('',#19858);
#5832=VERTEX_POINT('',#19860);
#5833=VERTEX_POINT('',#19864);
#5834=VERTEX_POINT('',#19866);
#5835=VERTEX_POINT('',#19870);
#5836=VERTEX_POINT('',#19872);
#5837=VERTEX_POINT('',#19876);
#5838=VERTEX_POINT('',#19878);
#5839=VERTEX_POINT('',#19882);
#5840=VERTEX_POINT('',#19884);
#5841=EDGE_CURVE('',#4892,#4892,#4379,.T.);
#5842=EDGE_CURVE('',#4892,#4893,#2665,.T.);
#5843=EDGE_CURVE('',#4893,#4893,#4380,.T.);
#5844=EDGE_CURVE('',#4894,#4894,#4381,.T.);
#5845=EDGE_CURVE('',#4894,#4895,#2666,.T.);
#5846=EDGE_CURVE('',#4895,#4895,#4382,.T.);
#5847=EDGE_CURVE('',#4896,#4896,#4383,.T.);
#5848=EDGE_CURVE('',#4896,#4897,#2667,.T.);
#5849=EDGE_CURVE('',#4897,#4897,#4384,.T.);
#5850=EDGE_CURVE('',#4898,#4898,#4385,.T.);
#5851=EDGE_CURVE('',#4898,#4899,#2668,.T.);
#5852=EDGE_CURVE('',#4899,#4899,#4386,.T.);
#5853=EDGE_CURVE('',#4900,#4900,#4387,.T.);
#5854=EDGE_CURVE('',#4900,#4901,#2669,.T.);
#5855=EDGE_CURVE('',#4901,#4901,#4388,.T.);
#5856=EDGE_CURVE('',#4902,#4902,#4389,.T.);
#5857=EDGE_CURVE('',#4902,#4903,#2670,.T.);
#5858=EDGE_CURVE('',#4903,#4903,#4390,.T.);
#5859=EDGE_CURVE('',#4904,#4904,#4391,.T.);
#5860=EDGE_CURVE('',#4904,#4905,#2671,.T.);
#5861=EDGE_CURVE('',#4905,#4905,#4392,.T.);
#5862=EDGE_CURVE('',#4906,#4906,#4393,.T.);
#5863=EDGE_CURVE('',#4906,#4907,#2672,.T.);
#5864=EDGE_CURVE('',#4907,#4907,#4394,.T.);
#5865=EDGE_CURVE('',#4908,#4908,#4395,.T.);
#5866=EDGE_CURVE('',#4908,#4909,#2673,.T.);
#5867=EDGE_CURVE('',#4909,#4909,#4396,.T.);
#5868=EDGE_CURVE('',#4910,#4910,#4397,.T.);
#5869=EDGE_CURVE('',#4910,#4911,#2674,.T.);
#5870=EDGE_CURVE('',#4911,#4911,#4398,.T.);
#5871=EDGE_CURVE('',#4912,#4912,#4399,.T.);
#5872=EDGE_CURVE('',#4912,#4913,#2675,.T.);
#5873=EDGE_CURVE('',#4913,#4913,#4400,.T.);
#5874=EDGE_CURVE('',#4914,#4914,#4401,.T.);
#5875=EDGE_CURVE('',#4914,#4915,#2676,.T.);
#5876=EDGE_CURVE('',#4915,#4915,#4402,.T.);
#5877=EDGE_CURVE('',#4916,#4916,#4403,.T.);
#5878=EDGE_CURVE('',#4916,#4917,#2677,.T.);
#5879=EDGE_CURVE('',#4917,#4917,#4404,.T.);
#5880=EDGE_CURVE('',#4918,#4918,#4405,.T.);
#5881=EDGE_CURVE('',#4918,#4919,#2678,.T.);
#5882=EDGE_CURVE('',#4919,#4919,#4406,.T.);
#5883=EDGE_CURVE('',#4920,#4920,#4407,.T.);
#5884=EDGE_CURVE('',#4920,#4921,#2679,.T.);
#5885=EDGE_CURVE('',#4921,#4921,#4408,.T.);
#5886=EDGE_CURVE('',#4922,#4922,#4409,.T.);
#5887=EDGE_CURVE('',#4922,#4923,#2680,.T.);
#5888=EDGE_CURVE('',#4923,#4923,#4410,.T.);
#5889=EDGE_CURVE('',#4924,#4924,#4411,.T.);
#5890=EDGE_CURVE('',#4924,#4925,#2681,.T.);
#5891=EDGE_CURVE('',#4925,#4925,#4412,.T.);
#5892=EDGE_CURVE('',#4926,#4926,#4413,.T.);
#5893=EDGE_CURVE('',#4926,#4927,#2682,.T.);
#5894=EDGE_CURVE('',#4927,#4927,#4414,.T.);
#5895=EDGE_CURVE('',#4928,#4928,#4415,.T.);
#5896=EDGE_CURVE('',#4928,#4929,#2683,.T.);
#5897=EDGE_CURVE('',#4929,#4929,#4416,.T.);
#5898=EDGE_CURVE('',#4930,#4930,#4417,.T.);
#5899=EDGE_CURVE('',#4930,#4931,#2684,.T.);
#5900=EDGE_CURVE('',#4931,#4931,#4418,.T.);
#5901=EDGE_CURVE('',#4932,#4933,#2685,.T.);
#5902=EDGE_CURVE('',#4933,#4934,#2686,.T.);
#5903=EDGE_CURVE('',#4935,#4934,#2687,.T.);
#5904=EDGE_CURVE('',#4932,#4935,#2688,.T.);
#5905=EDGE_CURVE('',#4936,#4932,#2689,.T.);
#5906=EDGE_CURVE('',#4937,#4935,#2690,.T.);
#5907=EDGE_CURVE('',#4936,#4937,#2691,.T.);
#5908=EDGE_CURVE('',#4938,#4936,#2692,.T.);
#5909=EDGE_CURVE('',#4939,#4937,#2693,.T.);
#5910=EDGE_CURVE('',#4938,#4939,#2694,.T.);
#5911=EDGE_CURVE('',#4933,#4938,#2695,.T.);
#5912=EDGE_CURVE('',#4934,#4939,#2696,.T.);
#5913=EDGE_CURVE('',#4940,#4941,#2697,.T.);
#5914=EDGE_CURVE('',#4942,#4940,#2698,.T.);
#5915=EDGE_CURVE('',#4943,#4942,#2699,.T.);
#5916=EDGE_CURVE('',#4941,#4943,#2700,.T.);
#5917=EDGE_CURVE('',#4942,#4944,#2701,.T.);
#5918=EDGE_CURVE('',#4944,#4945,#2702,.T.);
#5919=EDGE_CURVE('',#4945,#4943,#2703,.T.);
#5920=EDGE_CURVE('',#4940,#4946,#2704,.T.);
#5921=EDGE_CURVE('',#4946,#4944,#2705,.T.);
#5922=EDGE_CURVE('',#4947,#4946,#2706,.T.);
#5923=EDGE_CURVE('',#4945,#4947,#2707,.T.);
#5924=EDGE_CURVE('',#4947,#4941,#2708,.T.);
#5925=EDGE_CURVE('',#4948,#4949,#2709,.T.);
#5926=EDGE_CURVE('',#4949,#4950,#2710,.T.);
#5927=EDGE_CURVE('',#4951,#4950,#2711,.T.);
#5928=EDGE_CURVE('',#4948,#4951,#2712,.T.);
#5929=EDGE_CURVE('',#4952,#4953,#2713,.T.);
#5930=EDGE_CURVE('',#4953,#4948,#2714,.T.);
#5931=EDGE_CURVE('',#4952,#4951,#2715,.T.);
#5932=EDGE_CURVE('',#4954,#4952,#2716,.T.);
#5933=EDGE_CURVE('',#4950,#4954,#2717,.T.);
#5934=EDGE_CURVE('',#4955,#4954,#2718,.T.);
#5935=EDGE_CURVE('',#4949,#4955,#2719,.T.);
#5936=EDGE_CURVE('',#4953,#4955,#2720,.T.);
#5937=EDGE_CURVE('',#4956,#4957,#2721,.T.);
#5938=EDGE_CURVE('',#4958,#4956,#2722,.T.);
#5939=EDGE_CURVE('',#4959,#4958,#2723,.T.);
#5940=EDGE_CURVE('',#4957,#4959,#2724,.T.);
#5941=EDGE_CURVE('',#4958,#4960,#2725,.T.);
#5942=EDGE_CURVE('',#4960,#4961,#2726,.T.);
#5943=EDGE_CURVE('',#4961,#4959,#2727,.T.);
#5944=EDGE_CURVE('',#4956,#4962,#2728,.T.);
#5945=EDGE_CURVE('',#4962,#4960,#2729,.T.);
#5946=EDGE_CURVE('',#4963,#4962,#2730,.T.);
#5947=EDGE_CURVE('',#4961,#4963,#2731,.T.);
#5948=EDGE_CURVE('',#4963,#4957,#2732,.T.);
#5949=EDGE_CURVE('',#4964,#4965,#2733,.T.);
#5950=EDGE_CURVE('',#4965,#4966,#2734,.T.);
#5951=EDGE_CURVE('',#4967,#4966,#2735,.T.);
#5952=EDGE_CURVE('',#4964,#4967,#2736,.T.);
#5953=EDGE_CURVE('',#4968,#4969,#2737,.T.);
#5954=EDGE_CURVE('',#4969,#4964,#2738,.T.);
#5955=EDGE_CURVE('',#4968,#4967,#2739,.T.);
#5956=EDGE_CURVE('',#4970,#4968,#2740,.T.);
#5957=EDGE_CURVE('',#4966,#4970,#2741,.T.);
#5958=EDGE_CURVE('',#4971,#4970,#2742,.T.);
#5959=EDGE_CURVE('',#4965,#4971,#2743,.T.);
#5960=EDGE_CURVE('',#4969,#4971,#2744,.T.);
#5961=EDGE_CURVE('',#4972,#4972,#4419,.T.);
#5962=EDGE_CURVE('',#4972,#4973,#2745,.T.);
#5963=EDGE_CURVE('',#4973,#4973,#4420,.T.);
#5964=EDGE_CURVE('',#4974,#4974,#4421,.T.);
#5965=EDGE_CURVE('',#4974,#4975,#2746,.T.);
#5966=EDGE_CURVE('',#4975,#4975,#4422,.T.);
#5967=EDGE_CURVE('',#4976,#4976,#4423,.T.);
#5968=EDGE_CURVE('',#4976,#4977,#2747,.T.);
#5969=EDGE_CURVE('',#4977,#4977,#4424,.T.);
#5970=EDGE_CURVE('',#4978,#4978,#4425,.T.);
#5971=EDGE_CURVE('',#4978,#4979,#2748,.T.);
#5972=EDGE_CURVE('',#4979,#4979,#4426,.T.);
#5973=EDGE_CURVE('',#4980,#4980,#4427,.T.);
#5974=EDGE_CURVE('',#4980,#4981,#2749,.T.);
#5975=EDGE_CURVE('',#4981,#4981,#4428,.T.);
#5976=EDGE_CURVE('',#4982,#4982,#4429,.T.);
#5977=EDGE_CURVE('',#4982,#4983,#2750,.T.);
#5978=EDGE_CURVE('',#4983,#4983,#4430,.T.);
#5979=EDGE_CURVE('',#4984,#4984,#4431,.T.);
#5980=EDGE_CURVE('',#4984,#4985,#2751,.T.);
#5981=EDGE_CURVE('',#4985,#4985,#4432,.T.);
#5982=EDGE_CURVE('',#4986,#4986,#4433,.T.);
#5983=EDGE_CURVE('',#4986,#4987,#2752,.T.);
#5984=EDGE_CURVE('',#4987,#4987,#4434,.T.);
#5985=EDGE_CURVE('',#4988,#4988,#4435,.T.);
#5986=EDGE_CURVE('',#4988,#4989,#2753,.T.);
#5987=EDGE_CURVE('',#4989,#4989,#4436,.T.);
#5988=EDGE_CURVE('',#4990,#4991,#2754,.T.);
#5989=EDGE_CURVE('',#4992,#4990,#2755,.T.);
#5990=EDGE_CURVE('',#4992,#4993,#2756,.T.);
#5991=EDGE_CURVE('',#4991,#4993,#2757,.T.);
#5992=EDGE_CURVE('',#4994,#4995,#2758,.T.);
#5993=EDGE_CURVE('',#4996,#4994,#2759,.T.);
#5994=EDGE_CURVE('',#4997,#4996,#2760,.T.);
#5995=EDGE_CURVE('',#4995,#4997,#2761,.T.);
#5996=EDGE_CURVE('',#4997,#4998,#2762,.T.);
#5997=EDGE_CURVE('',#4999,#4996,#2763,.T.);
#5998=EDGE_CURVE('',#4998,#4999,#2764,.T.);
#5999=EDGE_CURVE('',#5000,#4992,#2765,.T.);
#6000=EDGE_CURVE('',#5000,#5001,#2766,.T.);
#6001=EDGE_CURVE('',#4993,#5001,#2767,.T.);
#6002=EDGE_CURVE('',#4990,#5002,#2768,.T.);
#6003=EDGE_CURVE('',#5003,#5002,#2769,.T.);
#6004=EDGE_CURVE('',#4995,#5003,#2770,.T.);
#6005=EDGE_CURVE('',#4998,#5000,#2771,.T.);
#6006=EDGE_CURVE('',#4991,#5004,#2772,.T.);
#6007=EDGE_CURVE('',#5002,#5004,#2773,.T.);
#6008=EDGE_CURVE('',#4994,#5005,#2774,.T.);
#6009=EDGE_CURVE('',#5004,#5005,#2775,.T.);
#6010=EDGE_CURVE('',#5001,#4999,#2776,.T.);
#6011=EDGE_CURVE('',#5005,#5003,#2777,.T.);
#6012=EDGE_CURVE('',#5006,#5006,#4437,.T.);
#6013=EDGE_CURVE('',#5006,#5007,#2778,.T.);
#6014=EDGE_CURVE('',#5007,#5007,#4438,.T.);
#6015=EDGE_CURVE('',#5008,#5008,#4439,.T.);
#6016=EDGE_CURVE('',#5008,#5009,#2779,.T.);
#6017=EDGE_CURVE('',#5009,#5009,#4440,.T.);
#6018=EDGE_CURVE('',#5010,#5011,#2780,.T.);
#6019=EDGE_CURVE('',#5012,#5010,#4441,.T.);
#6020=EDGE_CURVE('',#5013,#5012,#2781,.T.);
#6021=EDGE_CURVE('',#5011,#5013,#4442,.T.);
#6022=EDGE_CURVE('',#5014,#5015,#2782,.T.);
#6023=EDGE_CURVE('',#5016,#5014,#4443,.T.);
#6024=EDGE_CURVE('',#5017,#5016,#2783,.T.);
#6025=EDGE_CURVE('',#5015,#5017,#4444,.T.);
#6026=EDGE_CURVE('',#5018,#5019,#2784,.T.);
#6027=EDGE_CURVE('',#5020,#5018,#4445,.T.);
#6028=EDGE_CURVE('',#5021,#5020,#2785,.T.);
#6029=EDGE_CURVE('',#5019,#5021,#4446,.T.);
#6030=EDGE_CURVE('',#5022,#5023,#2786,.T.);
#6031=EDGE_CURVE('',#5024,#5022,#4447,.T.);
#6032=EDGE_CURVE('',#5025,#5024,#2787,.T.);
#6033=EDGE_CURVE('',#5023,#5025,#4448,.T.);
#6034=EDGE_CURVE('',#5024,#5010,#4449,.T.);
#6035=EDGE_CURVE('',#5020,#5022,#4450,.T.);
#6036=EDGE_CURVE('',#5016,#5018,#4451,.T.);
#6037=EDGE_CURVE('',#5012,#5014,#4452,.T.);
#6038=EDGE_CURVE('',#5026,#5026,#4453,.T.);
#6039=EDGE_CURVE('',#5021,#5023,#4454,.T.);
#6040=EDGE_CURVE('',#5017,#5019,#4455,.T.);
#6041=EDGE_CURVE('',#5025,#5011,#4456,.T.);
#6042=EDGE_CURVE('',#5013,#5015,#4457,.T.);
#6043=EDGE_CURVE('',#5027,#5027,#4458,.T.);
#6044=EDGE_CURVE('',#5027,#5028,#2788,.T.);
#6045=EDGE_CURVE('',#5028,#5028,#4459,.T.);
#6046=EDGE_CURVE('',#5029,#5029,#4460,.T.);
#6047=EDGE_CURVE('',#5029,#5026,#2789,.T.);
#6048=EDGE_CURVE('',#5030,#5031,#2790,.T.);
#6049=EDGE_CURVE('',#5032,#5030,#4461,.T.);
#6050=EDGE_CURVE('',#5033,#5032,#2791,.T.);
#6051=EDGE_CURVE('',#5031,#5033,#4462,.T.);
#6052=EDGE_CURVE('',#5034,#5035,#2792,.T.);
#6053=EDGE_CURVE('',#5036,#5034,#4463,.T.);
#6054=EDGE_CURVE('',#5037,#5036,#2793,.T.);
#6055=EDGE_CURVE('',#5035,#5037,#4464,.T.);
#6056=EDGE_CURVE('',#5038,#5039,#2794,.T.);
#6057=EDGE_CURVE('',#5040,#5038,#4465,.T.);
#6058=EDGE_CURVE('',#5041,#5040,#2795,.T.);
#6059=EDGE_CURVE('',#5039,#5041,#4466,.T.);
#6060=EDGE_CURVE('',#5042,#5043,#2796,.T.);
#6061=EDGE_CURVE('',#5044,#5042,#4467,.T.);
#6062=EDGE_CURVE('',#5045,#5044,#2797,.T.);
#6063=EDGE_CURVE('',#5043,#5045,#4468,.T.);
#6064=EDGE_CURVE('',#5044,#5030,#4469,.T.);
#6065=EDGE_CURVE('',#5040,#5042,#4470,.T.);
#6066=EDGE_CURVE('',#5036,#5038,#4471,.T.);
#6067=EDGE_CURVE('',#5032,#5034,#4472,.T.);
#6068=EDGE_CURVE('',#5046,#5046,#4473,.T.);
#6069=EDGE_CURVE('',#5041,#5043,#4474,.T.);
#6070=EDGE_CURVE('',#5037,#5039,#4475,.T.);
#6071=EDGE_CURVE('',#5045,#5031,#4476,.T.);
#6072=EDGE_CURVE('',#5033,#5035,#4477,.T.);
#6073=EDGE_CURVE('',#5046,#5047,#2798,.T.);
#6074=EDGE_CURVE('',#5047,#5047,#4478,.T.);
#6075=EDGE_CURVE('',#5048,#5048,#4479,.T.);
#6076=EDGE_CURVE('',#5049,#5049,#4480,.T.);
#6077=EDGE_CURVE('',#5049,#5048,#2799,.T.);
#6078=EDGE_CURVE('',#5050,#5050,#4481,.T.);
#6079=EDGE_CURVE('',#5050,#5051,#2800,.T.);
#6080=EDGE_CURVE('',#5051,#5051,#4482,.T.);
#6081=EDGE_CURVE('',#5052,#5052,#4483,.T.);
#6082=EDGE_CURVE('',#5052,#5053,#2801,.T.);
#6083=EDGE_CURVE('',#5053,#5053,#4484,.T.);
#6084=EDGE_CURVE('',#5054,#5054,#4485,.T.);
#6085=EDGE_CURVE('',#5054,#5055,#2802,.T.);
#6086=EDGE_CURVE('',#5055,#5055,#4486,.T.);
#6087=EDGE_CURVE('',#5056,#5056,#4487,.T.);
#6088=EDGE_CURVE('',#5056,#5057,#2803,.T.);
#6089=EDGE_CURVE('',#5057,#5057,#4488,.T.);
#6090=EDGE_CURVE('',#5058,#5058,#4489,.T.);
#6091=EDGE_CURVE('',#5058,#5059,#2804,.T.);
#6092=EDGE_CURVE('',#5059,#5059,#4490,.T.);
#6093=EDGE_CURVE('',#5060,#5060,#4491,.T.);
#6094=EDGE_CURVE('',#5060,#5061,#2805,.T.);
#6095=EDGE_CURVE('',#5061,#5061,#4492,.T.);
#6096=EDGE_CURVE('',#5062,#5062,#4493,.T.);
#6097=EDGE_CURVE('',#5062,#5063,#2806,.T.);
#6098=EDGE_CURVE('',#5063,#5063,#4494,.T.);
#6099=EDGE_CURVE('',#5064,#5064,#4495,.T.);
#6100=EDGE_CURVE('',#5064,#5065,#2807,.T.);
#6101=EDGE_CURVE('',#5065,#5065,#4496,.T.);
#6102=EDGE_CURVE('',#5066,#5066,#4497,.T.);
#6103=EDGE_CURVE('',#5066,#5067,#2808,.T.);
#6104=EDGE_CURVE('',#5067,#5067,#4498,.T.);
#6105=EDGE_CURVE('',#5068,#5069,#2809,.T.);
#6106=EDGE_CURVE('',#5070,#5068,#2810,.T.);
#6107=EDGE_CURVE('',#5070,#5071,#2811,.T.);
#6108=EDGE_CURVE('',#5069,#5071,#2812,.T.);
#6109=EDGE_CURVE('',#5072,#5073,#2813,.T.);
#6110=EDGE_CURVE('',#5074,#5072,#2814,.T.);
#6111=EDGE_CURVE('',#5075,#5074,#2815,.T.);
#6112=EDGE_CURVE('',#5073,#5075,#2816,.T.);
#6113=EDGE_CURVE('',#5075,#5076,#2817,.T.);
#6114=EDGE_CURVE('',#5077,#5074,#2818,.T.);
#6115=EDGE_CURVE('',#5076,#5077,#2819,.T.);
#6116=EDGE_CURVE('',#5078,#5070,#2820,.T.);
#6117=EDGE_CURVE('',#5078,#5079,#2821,.T.);
#6118=EDGE_CURVE('',#5071,#5079,#2822,.T.);
#6119=EDGE_CURVE('',#5068,#5080,#2823,.T.);
#6120=EDGE_CURVE('',#5081,#5080,#2824,.T.);
#6121=EDGE_CURVE('',#5073,#5081,#2825,.T.);
#6122=EDGE_CURVE('',#5076,#5078,#2826,.T.);
#6123=EDGE_CURVE('',#5069,#5082,#2827,.T.);
#6124=EDGE_CURVE('',#5080,#5082,#2828,.T.);
#6125=EDGE_CURVE('',#5072,#5083,#2829,.T.);
#6126=EDGE_CURVE('',#5082,#5083,#2830,.T.);
#6127=EDGE_CURVE('',#5079,#5077,#2831,.T.);
#6128=EDGE_CURVE('',#5083,#5081,#2832,.T.);
#6129=EDGE_CURVE('',#5084,#5084,#4499,.T.);
#6130=EDGE_CURVE('',#5084,#5085,#2833,.T.);
#6131=EDGE_CURVE('',#5085,#5085,#4500,.T.);
#6132=EDGE_CURVE('',#5086,#5086,#4501,.T.);
#6133=EDGE_CURVE('',#5086,#5087,#2834,.T.);
#6134=EDGE_CURVE('',#5087,#5087,#4502,.T.);
#6135=EDGE_CURVE('',#5088,#5089,#2835,.T.);
#6136=EDGE_CURVE('',#5090,#5088,#4503,.T.);
#6137=EDGE_CURVE('',#5091,#5090,#2836,.T.);
#6138=EDGE_CURVE('',#5089,#5091,#4504,.T.);
#6139=EDGE_CURVE('',#5092,#5093,#2837,.T.);
#6140=EDGE_CURVE('',#5094,#5092,#4505,.T.);
#6141=EDGE_CURVE('',#5095,#5094,#2838,.T.);
#6142=EDGE_CURVE('',#5093,#5095,#4506,.T.);
#6143=EDGE_CURVE('',#5096,#5097,#2839,.T.);
#6144=EDGE_CURVE('',#5098,#5096,#4507,.T.);
#6145=EDGE_CURVE('',#5099,#5098,#2840,.T.);
#6146=EDGE_CURVE('',#5097,#5099,#4508,.T.);
#6147=EDGE_CURVE('',#5100,#5101,#2841,.T.);
#6148=EDGE_CURVE('',#5102,#5100,#4509,.T.);
#6149=EDGE_CURVE('',#5103,#5102,#2842,.T.);
#6150=EDGE_CURVE('',#5101,#5103,#4510,.T.);
#6151=EDGE_CURVE('',#5102,#5088,#4511,.T.);
#6152=EDGE_CURVE('',#5098,#5100,#4512,.T.);
#6153=EDGE_CURVE('',#5094,#5096,#4513,.T.);
#6154=EDGE_CURVE('',#5090,#5092,#4514,.T.);
#6155=EDGE_CURVE('',#5104,#5104,#4515,.T.);
#6156=EDGE_CURVE('',#5099,#5101,#4516,.T.);
#6157=EDGE_CURVE('',#5095,#5097,#4517,.T.);
#6158=EDGE_CURVE('',#5103,#5089,#4518,.T.);
#6159=EDGE_CURVE('',#5091,#5093,#4519,.T.);
#6160=EDGE_CURVE('',#5105,#5105,#4520,.T.);
#6161=EDGE_CURVE('',#5105,#5106,#2843,.T.);
#6162=EDGE_CURVE('',#5106,#5106,#4521,.T.);
#6163=EDGE_CURVE('',#5107,#5107,#4522,.T.);
#6164=EDGE_CURVE('',#5107,#5104,#2844,.T.);
#6165=EDGE_CURVE('',#5108,#5109,#2845,.T.);
#6166=EDGE_CURVE('',#5110,#5108,#4523,.T.);
#6167=EDGE_CURVE('',#5111,#5110,#2846,.T.);
#6168=EDGE_CURVE('',#5109,#5111,#4524,.T.);
#6169=EDGE_CURVE('',#5112,#5113,#2847,.T.);
#6170=EDGE_CURVE('',#5114,#5112,#4525,.T.);
#6171=EDGE_CURVE('',#5115,#5114,#2848,.T.);
#6172=EDGE_CURVE('',#5113,#5115,#4526,.T.);
#6173=EDGE_CURVE('',#5116,#5117,#2849,.T.);
#6174=EDGE_CURVE('',#5118,#5116,#4527,.T.);
#6175=EDGE_CURVE('',#5119,#5118,#2850,.T.);
#6176=EDGE_CURVE('',#5117,#5119,#4528,.T.);
#6177=EDGE_CURVE('',#5120,#5121,#2851,.T.);
#6178=EDGE_CURVE('',#5122,#5120,#4529,.T.);
#6179=EDGE_CURVE('',#5123,#5122,#2852,.T.);
#6180=EDGE_CURVE('',#5121,#5123,#4530,.T.);
#6181=EDGE_CURVE('',#5122,#5108,#4531,.T.);
#6182=EDGE_CURVE('',#5118,#5120,#4532,.T.);
#6183=EDGE_CURVE('',#5114,#5116,#4533,.T.);
#6184=EDGE_CURVE('',#5110,#5112,#4534,.T.);
#6185=EDGE_CURVE('',#5124,#5124,#4535,.T.);
#6186=EDGE_CURVE('',#5119,#5121,#4536,.T.);
#6187=EDGE_CURVE('',#5115,#5117,#4537,.T.);
#6188=EDGE_CURVE('',#5123,#5109,#4538,.T.);
#6189=EDGE_CURVE('',#5111,#5113,#4539,.T.);
#6190=EDGE_CURVE('',#5124,#5125,#2853,.T.);
#6191=EDGE_CURVE('',#5125,#5125,#4540,.T.);
#6192=EDGE_CURVE('',#5126,#5126,#4541,.T.);
#6193=EDGE_CURVE('',#5127,#5127,#4542,.T.);
#6194=EDGE_CURVE('',#5127,#5126,#2854,.T.);
#6195=EDGE_CURVE('',#5128,#5129,#2855,.T.);
#6196=EDGE_CURVE('',#5130,#5128,#2856,.T.);
#6197=EDGE_CURVE('',#5131,#5130,#2857,.T.);
#6198=EDGE_CURVE('',#5131,#5129,#2858,.T.);
#6199=EDGE_CURVE('',#5132,#5133,#2859,.T.);
#6200=EDGE_CURVE('',#5134,#5132,#2860,.T.);
#6201=EDGE_CURVE('',#5135,#5134,#2861,.T.);
#6202=EDGE_CURVE('',#5133,#5135,#2862,.T.);
#6203=EDGE_CURVE('',#5136,#5137,#2863,.T.);
#6204=EDGE_CURVE('',#5138,#5136,#4543,.T.);
#6205=EDGE_CURVE('',#5139,#5138,#2864,.T.);
#6206=EDGE_CURVE('',#5137,#5139,#4544,.T.);
#6207=EDGE_CURVE('',#5129,#5132,#4545,.T.);
#6208=EDGE_CURVE('',#5133,#5128,#4546,.T.);
#6209=EDGE_CURVE('',#5134,#5131,#4547,.T.);
#6210=EDGE_CURVE('',#5130,#5135,#4548,.T.);
#6211=EDGE_CURVE('',#5139,#5140,#2865,.T.);
#6212=EDGE_CURVE('',#5141,#5140,#4549,.T.);
#6213=EDGE_CURVE('',#5137,#5141,#2866,.T.);
#6214=EDGE_CURVE('',#5138,#5142,#2867,.T.);
#6215=EDGE_CURVE('',#5140,#5142,#2868,.T.);
#6216=EDGE_CURVE('',#5143,#5141,#2869,.T.);
#6217=EDGE_CURVE('',#5136,#5143,#2870,.T.);
#6218=EDGE_CURVE('',#5142,#5143,#4550,.T.);
#6219=EDGE_CURVE('',#5144,#5145,#2871,.T.);
#6220=EDGE_CURVE('',#5146,#5144,#4551,.T.);
#6221=EDGE_CURVE('',#5147,#5146,#2872,.T.);
#6222=EDGE_CURVE('',#5145,#5147,#4552,.T.);
#6223=EDGE_CURVE('',#5148,#5149,#2873,.T.);
#6224=EDGE_CURVE('',#5150,#5148,#4553,.T.);
#6225=EDGE_CURVE('',#5151,#5150,#2874,.T.);
#6226=EDGE_CURVE('',#5149,#5151,#4554,.T.);
#6227=EDGE_CURVE('',#5145,#5148,#2875,.T.);
#6228=EDGE_CURVE('',#5150,#5147,#2876,.T.);
#6229=EDGE_CURVE('',#5152,#5152,#4555,.T.);
#6230=EDGE_CURVE('',#5153,#5154,#2877,.T.);
#6231=EDGE_CURVE('',#5155,#5153,#4556,.T.);
#6232=EDGE_CURVE('',#5156,#5155,#2878,.T.);
#6233=EDGE_CURVE('',#5154,#5156,#4557,.T.);
#6234=EDGE_CURVE('',#5157,#5158,#2879,.T.);
#6235=EDGE_CURVE('',#5159,#5157,#4558,.T.);
#6236=EDGE_CURVE('',#5160,#5159,#2880,.T.);
#6237=EDGE_CURVE('',#5158,#5160,#4559,.T.);
#6238=EDGE_CURVE('',#5154,#5157,#2881,.T.);
#6239=EDGE_CURVE('',#5159,#5156,#2882,.T.);
#6240=EDGE_CURVE('',#5161,#5161,#4560,.T.);
#6241=EDGE_CURVE('',#5162,#5146,#2883,.T.);
#6242=EDGE_CURVE('',#5163,#5162,#2884,.T.);
#6243=EDGE_CURVE('',#5163,#5164,#2885,.T.);
#6244=EDGE_CURVE('',#5164,#5165,#2886,.T.);
#6245=EDGE_CURVE('',#5165,#5166,#2887,.T.);
#6246=EDGE_CURVE('',#5166,#5167,#2888,.T.);
#6247=EDGE_CURVE('',#5167,#5168,#2889,.T.);
#6248=EDGE_CURVE('',#5168,#5169,#2890,.T.);
#6249=EDGE_CURVE('',#5160,#5169,#2891,.T.);
#6250=EDGE_CURVE('',#5151,#5155,#2892,.T.);
#6251=EDGE_CURVE('',#5169,#5170,#2893,.T.);
#6252=EDGE_CURVE('',#5170,#5158,#2894,.T.);
#6253=EDGE_CURVE('',#5144,#5171,#2895,.T.);
#6254=EDGE_CURVE('',#5171,#5162,#2896,.T.);
#6255=EDGE_CURVE('',#5153,#5149,#2897,.T.);
#6256=EDGE_CURVE('',#5172,#5172,#4561,.T.);
#6257=EDGE_CURVE('',#5172,#5152,#2898,.T.);
#6258=EDGE_CURVE('',#5173,#5173,#4562,.T.);
#6259=EDGE_CURVE('',#5173,#5161,#2899,.T.);
#6260=EDGE_CURVE('',#5166,#5174,#2900,.T.);
#6261=EDGE_CURVE('',#5175,#5174,#2901,.T.);
#6262=EDGE_CURVE('',#5167,#5175,#2902,.T.);
#6263=EDGE_CURVE('',#5176,#5164,#2903,.T.);
#6264=EDGE_CURVE('',#5177,#5176,#2904,.T.);
#6265=EDGE_CURVE('',#5177,#5165,#2905,.T.);
#6266=EDGE_CURVE('',#5174,#5177,#2906,.T.);
#6267=EDGE_CURVE('',#5178,#5170,#2907,.T.);
#6268=EDGE_CURVE('',#5178,#5175,#2908,.T.);
#6269=EDGE_CURVE('',#5176,#5179,#2909,.T.);
#6270=EDGE_CURVE('',#5179,#5171,#2910,.T.);
#6271=EDGE_CURVE('',#5179,#5163,#2911,.T.);
#6272=EDGE_CURVE('',#5168,#5178,#2912,.T.);
#6273=EDGE_CURVE('',#5180,#5181,#2913,.T.);
#6274=EDGE_CURVE('',#5182,#5180,#4563,.T.);
#6275=EDGE_CURVE('',#5183,#5182,#2914,.T.);
#6276=EDGE_CURVE('',#5181,#5183,#4564,.T.);
#6277=EDGE_CURVE('',#5184,#5185,#2915,.T.);
#6278=EDGE_CURVE('',#5186,#5184,#4565,.T.);
#6279=EDGE_CURVE('',#5187,#5186,#2916,.T.);
#6280=EDGE_CURVE('',#5185,#5187,#4566,.T.);
#6281=EDGE_CURVE('',#5181,#5184,#2917,.T.);
#6282=EDGE_CURVE('',#5186,#5183,#2918,.T.);
#6283=EDGE_CURVE('',#5188,#5188,#4567,.T.);
#6284=EDGE_CURVE('',#5189,#5190,#2919,.T.);
#6285=EDGE_CURVE('',#5191,#5189,#4568,.T.);
#6286=EDGE_CURVE('',#5192,#5191,#2920,.T.);
#6287=EDGE_CURVE('',#5190,#5192,#4569,.T.);
#6288=EDGE_CURVE('',#5193,#5194,#2921,.T.);
#6289=EDGE_CURVE('',#5195,#5193,#4570,.T.);
#6290=EDGE_CURVE('',#5196,#5195,#2922,.T.);
#6291=EDGE_CURVE('',#5194,#5196,#4571,.T.);
#6292=EDGE_CURVE('',#5190,#5193,#2923,.T.);
#6293=EDGE_CURVE('',#5195,#5192,#2924,.T.);
#6294=EDGE_CURVE('',#5197,#5197,#4572,.T.);
#6295=EDGE_CURVE('',#5198,#5182,#2925,.T.);
#6296=EDGE_CURVE('',#5199,#5198,#2926,.T.);
#6297=EDGE_CURVE('',#5199,#5200,#2927,.T.);
#6298=EDGE_CURVE('',#5200,#5201,#2928,.T.);
#6299=EDGE_CURVE('',#5201,#5202,#2929,.T.);
#6300=EDGE_CURVE('',#5202,#5203,#2930,.T.);
#6301=EDGE_CURVE('',#5203,#5204,#2931,.T.);
#6302=EDGE_CURVE('',#5204,#5205,#2932,.T.);
#6303=EDGE_CURVE('',#5196,#5205,#2933,.T.);
#6304=EDGE_CURVE('',#5187,#5191,#2934,.T.);
#6305=EDGE_CURVE('',#5205,#5206,#2935,.T.);
#6306=EDGE_CURVE('',#5206,#5194,#2936,.T.);
#6307=EDGE_CURVE('',#5180,#5207,#2937,.T.);
#6308=EDGE_CURVE('',#5207,#5198,#2938,.T.);
#6309=EDGE_CURVE('',#5189,#5185,#2939,.T.);
#6310=EDGE_CURVE('',#5208,#5208,#4573,.T.);
#6311=EDGE_CURVE('',#5208,#5188,#2940,.T.);
#6312=EDGE_CURVE('',#5209,#5209,#4574,.T.);
#6313=EDGE_CURVE('',#5209,#5197,#2941,.T.);
#6314=EDGE_CURVE('',#5202,#5210,#2942,.T.);
#6315=EDGE_CURVE('',#5211,#5210,#2943,.T.);
#6316=EDGE_CURVE('',#5203,#5211,#2944,.T.);
#6317=EDGE_CURVE('',#5212,#5200,#2945,.T.);
#6318=EDGE_CURVE('',#5213,#5212,#2946,.T.);
#6319=EDGE_CURVE('',#5213,#5201,#2947,.T.);
#6320=EDGE_CURVE('',#5210,#5213,#2948,.T.);
#6321=EDGE_CURVE('',#5214,#5206,#2949,.T.);
#6322=EDGE_CURVE('',#5214,#5211,#2950,.T.);
#6323=EDGE_CURVE('',#5212,#5215,#2951,.T.);
#6324=EDGE_CURVE('',#5215,#5207,#2952,.T.);
#6325=EDGE_CURVE('',#5215,#5199,#2953,.T.);
#6326=EDGE_CURVE('',#5204,#5214,#2954,.T.);
#6327=EDGE_CURVE('',#5216,#5217,#4575,.T.);
#6328=EDGE_CURVE('',#5217,#5216,#4576,.T.);
#6329=EDGE_CURVE('',#5217,#5218,#4577,.T.);
#6330=EDGE_CURVE('',#5219,#5218,#4578,.T.);
#6331=EDGE_CURVE('',#5218,#5219,#4579,.T.);
#6332=EDGE_CURVE('',#5219,#5220,#2955,.T.);
#6333=EDGE_CURVE('',#5220,#5220,#4580,.T.);
#6334=EDGE_CURVE('',#5221,#5221,#4581,.T.);
#6335=EDGE_CURVE('',#5221,#5222,#2956,.T.);
#6336=EDGE_CURVE('',#5222,#5222,#4582,.T.);
#6337=EDGE_CURVE('',#5222,#5223,#2957,.T.);
#6338=EDGE_CURVE('',#5223,#5223,#4583,.T.);
#6339=EDGE_CURVE('',#5224,#5224,#4584,.T.);
#6340=EDGE_CURVE('',#5224,#5216,#2958,.T.);
#6341=EDGE_CURVE('',#5225,#5225,#4585,.T.);
#6342=EDGE_CURVE('',#5225,#5221,#2959,.T.);
#6343=EDGE_CURVE('',#5226,#5227,#4586,.T.);
#6344=EDGE_CURVE('',#5227,#5226,#4587,.T.);
#6345=EDGE_CURVE('',#5227,#5228,#4588,.T.);
#6346=EDGE_CURVE('',#5229,#5228,#4589,.T.);
#6347=EDGE_CURVE('',#5228,#5229,#4590,.T.);
#6348=EDGE_CURVE('',#5230,#5230,#4591,.T.);
#6349=EDGE_CURVE('',#5230,#5229,#2960,.T.);
#6350=EDGE_CURVE('',#5231,#5231,#4592,.T.);
#6351=EDGE_CURVE('',#5232,#5232,#4593,.T.);
#6352=EDGE_CURVE('',#5233,#5233,#4594,.T.);
#6353=EDGE_CURVE('',#5233,#5231,#2961,.T.);
#6354=EDGE_CURVE('',#5234,#5234,#4595,.T.);
#6355=EDGE_CURVE('',#5234,#5233,#2962,.T.);
#6356=EDGE_CURVE('',#5235,#5235,#4596,.T.);
#6357=EDGE_CURVE('',#5235,#5234,#2963,.T.);
#6358=EDGE_CURVE('',#5226,#5232,#2964,.T.);
#6359=EDGE_CURVE('',#5236,#5237,#4597,.T.);
#6360=EDGE_CURVE('',#5238,#5239,#4598,.T.);
#6361=EDGE_CURVE('',#5240,#5241,#4599,.T.);
#6362=EDGE_CURVE('',#5242,#5243,#4600,.T.);
#6363=EDGE_CURVE('',#5244,#5245,#4601,.T.);
#6364=EDGE_CURVE('',#5246,#5247,#4602,.T.);
#6365=EDGE_CURVE('',#5248,#5249,#4603,.T.);
#6366=EDGE_CURVE('',#5250,#5251,#4604,.T.);
#6367=EDGE_CURVE('',#5252,#5253,#441,.T.);
#6368=EDGE_CURVE('',#5254,#5252,#4605,.T.);
#6369=EDGE_CURVE('',#5255,#5254,#442,.T.);
#6370=EDGE_CURVE('',#5253,#5255,#4606,.T.);
#6371=EDGE_CURVE('',#5256,#5254,#4607,.T.);
#6372=EDGE_CURVE('',#5256,#5257,#443,.T.);
#6373=EDGE_CURVE('',#5258,#5257,#4608,.T.);
#6374=EDGE_CURVE('',#5258,#5259,#444,.T.);
#6375=EDGE_CURVE('',#5260,#5259,#4609,.T.);
#6376=EDGE_CURVE('',#5260,#5261,#445,.T.);
#6377=EDGE_CURVE('',#5261,#5262,#2965,.T.);
#6378=EDGE_CURVE('',#5262,#5262,#4610,.T.);
#6379=EDGE_CURVE('',#5261,#5263,#446,.T.);
#6380=EDGE_CURVE('',#5264,#5263,#4611,.T.);
#6381=EDGE_CURVE('',#5264,#5265,#447,.T.);
#6382=EDGE_CURVE('',#5266,#5265,#4612,.T.);
#6383=EDGE_CURVE('',#5266,#5267,#448,.T.);
#6384=EDGE_CURVE('',#5268,#5267,#4613,.T.);
#6385=EDGE_CURVE('',#5268,#5269,#449,.T.);
#6386=EDGE_CURVE('',#5270,#5269,#4614,.T.);
#6387=EDGE_CURVE('',#5270,#5271,#450,.T.);
#6388=EDGE_CURVE('',#5255,#5271,#4615,.T.);
#6389=EDGE_CURVE('',#5252,#5272,#4616,.T.);
#6390=EDGE_CURVE('',#5272,#5256,#4617,.T.);
#6391=EDGE_CURVE('',#5273,#5272,#451,.T.);
#6392=EDGE_CURVE('',#5257,#5273,#4618,.T.);
#6393=EDGE_CURVE('',#5273,#5274,#4619,.T.);
#6394=EDGE_CURVE('',#5274,#5258,#4620,.T.);
#6395=EDGE_CURVE('',#5275,#5274,#452,.T.);
#6396=EDGE_CURVE('',#5259,#5275,#4621,.T.);
#6397=EDGE_CURVE('',#5275,#5276,#4622,.T.);
#6398=EDGE_CURVE('',#5276,#5260,#4623,.T.);
#6399=EDGE_CURVE('',#5277,#5278,#453,.T.);
#6400=EDGE_CURVE('',#5263,#5277,#4624,.T.);
#6401=EDGE_CURVE('',#5278,#5276,#454,.T.);
#6402=EDGE_CURVE('',#5277,#5279,#4625,.T.);
#6403=EDGE_CURVE('',#5279,#5264,#4626,.T.);
#6404=EDGE_CURVE('',#5280,#5279,#455,.T.);
#6405=EDGE_CURVE('',#5265,#5280,#4627,.T.);
#6406=EDGE_CURVE('',#5280,#5281,#4628,.T.);
#6407=EDGE_CURVE('',#5281,#5266,#4629,.T.);
#6408=EDGE_CURVE('',#5282,#5281,#456,.T.);
#6409=EDGE_CURVE('',#5267,#5282,#4630,.T.);
#6410=EDGE_CURVE('',#5282,#5283,#4631,.T.);
#6411=EDGE_CURVE('',#5283,#5268,#4632,.T.);
#6412=EDGE_CURVE('',#5284,#5283,#457,.T.);
#6413=EDGE_CURVE('',#5269,#5284,#4633,.T.);
#6414=EDGE_CURVE('',#5285,#5285,#4634,.T.);
#6415=EDGE_CURVE('',#5285,#5278,#2966,.T.);
#6416=EDGE_CURVE('',#5286,#5253,#4635,.T.);
#6417=EDGE_CURVE('',#5286,#5287,#458,.T.);
#6418=EDGE_CURVE('',#5284,#5287,#4636,.T.);
#6419=EDGE_CURVE('',#5271,#5286,#4637,.T.);
#6420=EDGE_CURVE('',#5287,#5270,#4638,.T.);
#6421=EDGE_CURVE('',#5288,#5288,#4639,.T.);
#6422=EDGE_CURVE('',#5289,#5289,#4640,.T.);
#6423=EDGE_CURVE('',#5290,#5290,#4641,.T.);
#6424=EDGE_CURVE('',#5290,#5288,#2967,.T.);
#6425=EDGE_CURVE('',#5291,#5291,#4642,.T.);
#6426=EDGE_CURVE('',#5291,#5289,#2968,.T.);
#6427=EDGE_CURVE('',#5292,#5292,#4643,.T.);
#6428=EDGE_CURVE('',#5293,#5293,#4644,.T.);
#6429=EDGE_CURVE('',#5294,#5294,#4645,.T.);
#6430=EDGE_CURVE('',#5294,#5292,#2969,.T.);
#6431=EDGE_CURVE('',#5295,#5295,#4646,.T.);
#6432=EDGE_CURVE('',#5295,#5293,#2970,.T.);
#6433=EDGE_CURVE('',#5296,#5297,#2971,.T.);
#6434=EDGE_CURVE('',#5296,#5298,#2972,.T.);
#6435=EDGE_CURVE('',#5299,#5298,#2973,.T.);
#6436=EDGE_CURVE('',#5297,#5299,#2974,.T.);
#6437=EDGE_CURVE('',#5300,#5296,#2975,.T.);
#6438=EDGE_CURVE('',#5300,#5301,#2976,.T.);
#6439=EDGE_CURVE('',#5298,#5301,#2977,.T.);
#6440=EDGE_CURVE('',#5302,#5300,#2978,.T.);
#6441=EDGE_CURVE('',#5302,#5303,#2979,.T.);
#6442=EDGE_CURVE('',#5301,#5303,#2980,.T.);
#6443=EDGE_CURVE('',#5304,#5302,#2981,.T.);
#6444=EDGE_CURVE('',#5304,#5305,#2982,.T.);
#6445=EDGE_CURVE('',#5303,#5305,#2983,.T.);
#6446=EDGE_CURVE('',#5306,#5304,#2984,.T.);
#6447=EDGE_CURVE('',#5306,#5307,#2985,.T.);
#6448=EDGE_CURVE('',#5305,#5307,#2986,.T.);
#6449=EDGE_CURVE('',#5308,#5306,#2987,.T.);
#6450=EDGE_CURVE('',#5308,#5309,#2988,.T.);
#6451=EDGE_CURVE('',#5307,#5309,#2989,.T.);
#6452=EDGE_CURVE('',#5310,#5308,#2990,.T.);
#6453=EDGE_CURVE('',#5310,#5311,#2991,.T.);
#6454=EDGE_CURVE('',#5309,#5311,#2992,.T.);
#6455=EDGE_CURVE('',#5312,#5310,#2993,.T.);
#6456=EDGE_CURVE('',#5312,#5313,#2994,.T.);
#6457=EDGE_CURVE('',#5311,#5313,#2995,.T.);
#6458=EDGE_CURVE('',#5314,#5312,#2996,.T.);
#6459=EDGE_CURVE('',#5315,#5314,#2997,.T.);
#6460=EDGE_CURVE('',#5313,#5315,#2998,.T.);
#6461=EDGE_CURVE('',#5316,#5317,#2999,.T.);
#6462=EDGE_CURVE('',#5316,#5318,#3000,.T.);
#6463=EDGE_CURVE('',#5319,#5318,#3001,.T.);
#6464=EDGE_CURVE('',#5317,#5319,#3002,.T.);
#6465=EDGE_CURVE('',#5320,#5316,#3003,.T.);
#6466=EDGE_CURVE('',#5320,#5321,#3004,.T.);
#6467=EDGE_CURVE('',#5318,#5321,#3005,.T.);
#6468=EDGE_CURVE('',#5322,#5320,#3006,.T.);
#6469=EDGE_CURVE('',#5322,#5323,#3007,.T.);
#6470=EDGE_CURVE('',#5321,#5323,#3008,.T.);
#6471=EDGE_CURVE('',#5324,#5322,#3009,.T.);
#6472=EDGE_CURVE('',#5324,#5325,#3010,.T.);
#6473=EDGE_CURVE('',#5323,#5325,#3011,.T.);
#6474=EDGE_CURVE('',#5326,#5324,#3012,.T.);
#6475=EDGE_CURVE('',#5326,#5327,#3013,.T.);
#6476=EDGE_CURVE('',#5325,#5327,#3014,.T.);
#6477=EDGE_CURVE('',#5328,#5326,#3015,.T.);
#6478=EDGE_CURVE('',#5328,#5329,#3016,.T.);
#6479=EDGE_CURVE('',#5327,#5329,#3017,.T.);
#6480=EDGE_CURVE('',#5330,#5328,#3018,.T.);
#6481=EDGE_CURVE('',#5330,#5331,#3019,.T.);
#6482=EDGE_CURVE('',#5329,#5331,#3020,.T.);
#6483=EDGE_CURVE('',#5332,#5330,#3021,.T.);
#6484=EDGE_CURVE('',#5332,#5333,#3022,.T.);
#6485=EDGE_CURVE('',#5331,#5333,#3023,.T.);
#6486=EDGE_CURVE('',#5334,#5332,#3024,.T.);
#6487=EDGE_CURVE('',#5335,#5334,#3025,.T.);
#6488=EDGE_CURVE('',#5333,#5335,#3026,.T.);
#6489=EDGE_CURVE('',#5336,#5337,#3027,.T.);
#6490=EDGE_CURVE('',#5336,#5338,#3028,.T.);
#6491=EDGE_CURVE('',#5339,#5338,#3029,.T.);
#6492=EDGE_CURVE('',#5337,#5339,#3030,.T.);
#6493=EDGE_CURVE('',#5340,#5336,#3031,.T.);
#6494=EDGE_CURVE('',#5340,#5341,#3032,.T.);
#6495=EDGE_CURVE('',#5338,#5341,#3033,.T.);
#6496=EDGE_CURVE('',#5342,#5340,#3034,.T.);
#6497=EDGE_CURVE('',#5342,#5343,#3035,.T.);
#6498=EDGE_CURVE('',#5341,#5343,#3036,.T.);
#6499=EDGE_CURVE('',#5344,#5342,#3037,.T.);
#6500=EDGE_CURVE('',#5344,#5345,#3038,.T.);
#6501=EDGE_CURVE('',#5343,#5345,#3039,.T.);
#6502=EDGE_CURVE('',#5346,#5344,#3040,.T.);
#6503=EDGE_CURVE('',#5346,#5347,#3041,.T.);
#6504=EDGE_CURVE('',#5345,#5347,#3042,.T.);
#6505=EDGE_CURVE('',#5348,#5346,#3043,.T.);
#6506=EDGE_CURVE('',#5348,#5349,#3044,.T.);
#6507=EDGE_CURVE('',#5347,#5349,#3045,.T.);
#6508=EDGE_CURVE('',#5350,#5348,#3046,.T.);
#6509=EDGE_CURVE('',#5350,#5351,#3047,.T.);
#6510=EDGE_CURVE('',#5349,#5351,#3048,.T.);
#6511=EDGE_CURVE('',#5352,#5350,#3049,.T.);
#6512=EDGE_CURVE('',#5352,#5353,#3050,.T.);
#6513=EDGE_CURVE('',#5351,#5353,#3051,.T.);
#6514=EDGE_CURVE('',#5354,#5352,#3052,.T.);
#6515=EDGE_CURVE('',#5355,#5354,#3053,.T.);
#6516=EDGE_CURVE('',#5353,#5355,#3054,.T.);
#6517=EDGE_CURVE('',#5356,#5357,#3055,.T.);
#6518=EDGE_CURVE('',#5356,#5358,#3056,.T.);
#6519=EDGE_CURVE('',#5359,#5358,#3057,.T.);
#6520=EDGE_CURVE('',#5357,#5359,#3058,.T.);
#6521=EDGE_CURVE('',#5360,#5356,#3059,.T.);
#6522=EDGE_CURVE('',#5360,#5361,#3060,.T.);
#6523=EDGE_CURVE('',#5358,#5361,#3061,.T.);
#6524=EDGE_CURVE('',#5362,#5360,#3062,.T.);
#6525=EDGE_CURVE('',#5362,#5363,#3063,.T.);
#6526=EDGE_CURVE('',#5361,#5363,#3064,.T.);
#6527=EDGE_CURVE('',#5364,#5362,#3065,.T.);
#6528=EDGE_CURVE('',#5364,#5365,#3066,.T.);
#6529=EDGE_CURVE('',#5363,#5365,#3067,.T.);
#6530=EDGE_CURVE('',#5366,#5364,#3068,.T.);
#6531=EDGE_CURVE('',#5366,#5367,#3069,.T.);
#6532=EDGE_CURVE('',#5365,#5367,#3070,.T.);
#6533=EDGE_CURVE('',#5368,#5366,#3071,.T.);
#6534=EDGE_CURVE('',#5368,#5369,#3072,.T.);
#6535=EDGE_CURVE('',#5367,#5369,#3073,.T.);
#6536=EDGE_CURVE('',#5370,#5368,#3074,.T.);
#6537=EDGE_CURVE('',#5370,#5371,#3075,.T.);
#6538=EDGE_CURVE('',#5369,#5371,#3076,.T.);
#6539=EDGE_CURVE('',#5372,#5370,#3077,.T.);
#6540=EDGE_CURVE('',#5372,#5373,#3078,.T.);
#6541=EDGE_CURVE('',#5371,#5373,#3079,.T.);
#6542=EDGE_CURVE('',#5374,#5372,#3080,.T.);
#6543=EDGE_CURVE('',#5375,#5374,#3081,.T.);
#6544=EDGE_CURVE('',#5373,#5375,#3082,.T.);
#6545=EDGE_CURVE('',#5376,#5376,#4647,.T.);
#6546=EDGE_CURVE('',#5376,#5377,#3083,.T.);
#6547=EDGE_CURVE('',#5377,#5377,#4648,.T.);
#6548=EDGE_CURVE('',#5314,#5378,#3084,.T.);
#6549=EDGE_CURVE('',#5378,#5379,#3085,.T.);
#6550=EDGE_CURVE('',#5315,#5379,#3086,.T.);
#6551=EDGE_CURVE('',#5380,#5299,#3087,.T.);
#6552=EDGE_CURVE('',#5381,#5380,#3088,.T.);
#6553=EDGE_CURVE('',#5381,#5297,#3089,.T.);
#6554=EDGE_CURVE('',#5334,#5381,#3090,.T.);
#6555=EDGE_CURVE('',#5335,#5380,#3091,.T.);
#6556=EDGE_CURVE('',#5382,#5319,#3092,.T.);
#6557=EDGE_CURVE('',#5383,#5382,#3093,.T.);
#6558=EDGE_CURVE('',#5383,#5317,#3094,.T.);
#6559=EDGE_CURVE('',#5354,#5383,#3095,.T.);
#6560=EDGE_CURVE('',#5355,#5382,#3096,.T.);
#6561=EDGE_CURVE('',#5384,#5339,#3097,.T.);
#6562=EDGE_CURVE('',#5385,#5384,#3098,.T.);
#6563=EDGE_CURVE('',#5385,#5337,#3099,.T.);
#6564=EDGE_CURVE('',#5374,#5385,#3100,.T.);
#6565=EDGE_CURVE('',#5375,#5384,#3101,.T.);
#6566=EDGE_CURVE('',#5379,#5359,#3102,.T.);
#6567=EDGE_CURVE('',#5378,#5357,#3103,.T.);
#6568=EDGE_CURVE('',#5386,#5387,#3104,.T.);
#6569=EDGE_CURVE('',#5388,#5386,#3105,.T.);
#6570=EDGE_CURVE('',#5389,#5388,#3106,.T.);
#6571=EDGE_CURVE('',#5387,#5389,#3107,.T.);
#6572=EDGE_CURVE('',#5388,#5390,#3108,.T.);
#6573=EDGE_CURVE('',#5391,#5390,#3109,.T.);
#6574=EDGE_CURVE('',#5389,#5391,#3110,.T.);
#6575=EDGE_CURVE('',#5390,#5392,#3111,.T.);
#6576=EDGE_CURVE('',#5392,#5393,#3112,.T.);
#6577=EDGE_CURVE('',#5393,#5391,#3113,.T.);
#6578=EDGE_CURVE('',#5394,#5394,#4649,.T.);
#6579=EDGE_CURVE('',#5395,#5386,#3114,.T.);
#6580=EDGE_CURVE('',#5396,#5395,#3115,.T.);
#6581=EDGE_CURVE('',#5396,#5397,#3116,.T.);
#6582=EDGE_CURVE('',#5398,#5397,#3117,.T.);
#6583=EDGE_CURVE('',#5398,#5399,#3118,.T.);
#6584=EDGE_CURVE('',#5399,#5400,#3119,.T.);
#6585=EDGE_CURVE('',#5400,#5392,#3120,.T.);
#6586=EDGE_CURVE('',#5400,#5401,#3121,.T.);
#6587=EDGE_CURVE('',#5401,#5393,#3122,.T.);
#6588=EDGE_CURVE('',#5402,#5399,#3123,.T.);
#6589=EDGE_CURVE('',#5401,#5402,#3124,.T.);
#6590=EDGE_CURVE('',#5403,#5402,#3125,.T.);
#6591=EDGE_CURVE('',#5404,#5403,#3126,.T.);
#6592=EDGE_CURVE('',#5404,#5405,#3127,.T.);
#6593=EDGE_CURVE('',#5406,#5405,#3128,.T.);
#6594=EDGE_CURVE('',#5406,#5387,#3129,.T.);
#6595=EDGE_CURVE('',#5403,#5398,#3130,.T.);
#6596=EDGE_CURVE('',#5397,#5407,#3131,.T.);
#6597=EDGE_CURVE('',#5407,#5408,#19,.T.);
#6598=EDGE_CURVE('',#5408,#5404,#3132,.T.);
#6599=EDGE_CURVE('',#5409,#5407,#4650,.F.);
#6600=EDGE_CURVE('',#5409,#5394,#3133,.T.);
#6601=EDGE_CURVE('',#5410,#5409,#4651,.F.);
#6602=EDGE_CURVE('',#5411,#5410,#20,.T.);
#6603=EDGE_CURVE('',#5408,#5411,#4652,.F.);
#6604=EDGE_CURVE('',#5410,#5396,#3134,.T.);
#6605=EDGE_CURVE('',#5405,#5411,#3135,.T.);
#6606=EDGE_CURVE('',#5395,#5406,#3136,.T.);
#6607=EDGE_CURVE('',#5412,#5413,#3137,.T.);
#6608=EDGE_CURVE('',#5413,#5414,#3138,.T.);
#6609=EDGE_CURVE('',#5414,#5415,#3139,.T.);
#6610=EDGE_CURVE('',#5412,#5415,#3140,.T.);
#6611=EDGE_CURVE('',#5413,#5416,#3141,.T.);
#6612=EDGE_CURVE('',#5416,#5417,#3142,.T.);
#6613=EDGE_CURVE('',#5417,#5414,#3143,.T.);
#6614=EDGE_CURVE('',#5416,#5418,#3144,.T.);
#6615=EDGE_CURVE('',#5418,#5419,#3145,.T.);
#6616=EDGE_CURVE('',#5419,#5417,#3146,.T.);
#6617=EDGE_CURVE('',#5418,#5420,#3147,.T.);
#6618=EDGE_CURVE('',#5420,#5421,#3148,.T.);
#6619=EDGE_CURVE('',#5421,#5419,#3149,.T.);
#6620=EDGE_CURVE('',#5420,#5422,#3150,.T.);
#6621=EDGE_CURVE('',#5422,#5423,#3151,.T.);
#6622=EDGE_CURVE('',#5423,#5421,#3152,.T.);
#6623=EDGE_CURVE('',#5422,#5412,#3153,.T.);
#6624=EDGE_CURVE('',#5415,#5423,#3154,.T.);
#6625=EDGE_CURVE('',#5424,#5424,#4653,.T.);
#6626=EDGE_CURVE('',#5425,#5425,#4654,.T.);
#6627=EDGE_CURVE('',#5426,#5426,#4655,.T.);
#6628=EDGE_CURVE('',#5426,#5425,#3155,.T.);
#6629=EDGE_CURVE('',#5427,#5427,#4656,.T.);
#6630=EDGE_CURVE('',#5427,#5426,#3156,.T.);
#6631=EDGE_CURVE('',#5428,#5428,#4657,.T.);
#6632=EDGE_CURVE('',#5428,#5427,#3157,.T.);
#6633=EDGE_CURVE('',#5429,#5429,#4658,.T.);
#6634=EDGE_CURVE('',#5430,#5430,#4659,.F.);
#6635=EDGE_CURVE('',#5430,#5429,#3158,.T.);
#6636=EDGE_CURVE('',#5424,#5430,#3159,.T.);
#6637=EDGE_CURVE('',#5431,#5431,#4660,.T.);
#6638=EDGE_CURVE('',#5431,#5432,#3160,.T.);
#6639=EDGE_CURVE('',#5432,#5432,#4661,.T.);
#6640=EDGE_CURVE('',#5433,#5433,#4662,.T.);
#6641=EDGE_CURVE('',#5434,#5434,#4663,.T.);
#6642=EDGE_CURVE('',#5434,#5435,#3161,.T.);
#6643=EDGE_CURVE('',#5435,#5435,#4664,.T.);
#6644=EDGE_CURVE('',#5436,#5436,#4665,.T.);
#6645=EDGE_CURVE('',#5437,#5437,#4666,.T.);
#6646=EDGE_CURVE('',#5437,#5438,#3162,.T.);
#6647=EDGE_CURVE('',#5438,#5438,#4667,.T.);
#6648=EDGE_CURVE('',#5439,#5439,#4668,.T.);
#6649=EDGE_CURVE('',#5440,#5440,#4669,.T.);
#6650=EDGE_CURVE('',#5440,#5441,#3163,.T.);
#6651=EDGE_CURVE('',#5441,#5441,#4670,.T.);
#6652=EDGE_CURVE('',#5442,#5442,#4671,.T.);
#6653=EDGE_CURVE('',#5443,#5443,#4672,.T.);
#6654=EDGE_CURVE('',#5443,#5433,#3164,.T.);
#6655=EDGE_CURVE('',#5444,#5444,#4673,.T.);
#6656=EDGE_CURVE('',#5444,#5436,#3165,.T.);
#6657=EDGE_CURVE('',#5445,#5445,#4674,.T.);
#6658=EDGE_CURVE('',#5445,#5439,#3166,.T.);
#6659=EDGE_CURVE('',#5446,#5446,#4675,.T.);
#6660=EDGE_CURVE('',#5446,#5442,#3167,.T.);
#6661=EDGE_CURVE('',#5447,#5448,#3168,.T.);
#6662=EDGE_CURVE('',#5448,#5449,#3169,.T.);
#6663=EDGE_CURVE('',#5450,#5449,#3170,.T.);
#6664=EDGE_CURVE('',#5447,#5450,#3171,.T.);
#6665=EDGE_CURVE('',#5451,#5447,#3172,.T.);
#6666=EDGE_CURVE('',#5452,#5450,#3173,.T.);
#6667=EDGE_CURVE('',#5451,#5452,#3174,.T.);
#6668=EDGE_CURVE('',#5453,#5451,#3175,.T.);
#6669=EDGE_CURVE('',#5454,#5452,#3176,.T.);
#6670=EDGE_CURVE('',#5453,#5454,#3177,.T.);
#6671=EDGE_CURVE('',#5455,#5453,#3178,.T.);
#6672=EDGE_CURVE('',#5456,#5454,#3179,.T.);
#6673=EDGE_CURVE('',#5455,#5456,#3180,.T.);
#6674=EDGE_CURVE('',#5457,#5455,#3181,.T.);
#6675=EDGE_CURVE('',#5458,#5456,#3182,.T.);
#6676=EDGE_CURVE('',#5457,#5458,#3183,.T.);
#6677=EDGE_CURVE('',#5459,#5457,#3184,.T.);
#6678=EDGE_CURVE('',#5460,#5458,#3185,.T.);
#6679=EDGE_CURVE('',#5459,#5460,#3186,.T.);
#6680=EDGE_CURVE('',#5461,#5459,#3187,.T.);
#6681=EDGE_CURVE('',#5462,#5460,#3188,.T.);
#6682=EDGE_CURVE('',#5461,#5462,#3189,.T.);
#6683=EDGE_CURVE('',#5463,#5461,#3190,.T.);
#6684=EDGE_CURVE('',#5464,#5462,#3191,.T.);
#6685=EDGE_CURVE('',#5463,#5464,#3192,.T.);
#6686=EDGE_CURVE('',#5465,#5463,#3193,.T.);
#6687=EDGE_CURVE('',#5466,#5464,#3194,.T.);
#6688=EDGE_CURVE('',#5465,#5466,#3195,.T.);
#6689=EDGE_CURVE('',#5467,#5465,#3196,.T.);
#6690=EDGE_CURVE('',#5468,#5466,#3197,.T.);
#6691=EDGE_CURVE('',#5467,#5468,#3198,.T.);
#6692=EDGE_CURVE('',#5469,#5467,#3199,.T.);
#6693=EDGE_CURVE('',#5470,#5468,#3200,.T.);
#6694=EDGE_CURVE('',#5469,#5470,#3201,.T.);
#6695=EDGE_CURVE('',#5448,#5469,#3202,.T.);
#6696=EDGE_CURVE('',#5449,#5470,#3203,.T.);
#6697=EDGE_CURVE('',#5471,#5471,#4676,.T.);
#6698=EDGE_CURVE('',#5471,#5472,#3204,.T.);
#6699=EDGE_CURVE('',#5472,#5472,#4677,.T.);
#6700=EDGE_CURVE('',#5473,#5473,#4678,.T.);
#6701=EDGE_CURVE('',#5474,#5474,#4679,.T.);
#6702=EDGE_CURVE('',#5475,#5475,#4680,.T.);
#6703=EDGE_CURVE('',#5476,#5476,#4681,.T.);
#6704=EDGE_CURVE('',#5473,#5475,#3205,.T.);
#6705=EDGE_CURVE('',#5476,#5477,#3206,.T.);
#6706=EDGE_CURVE('',#5477,#5477,#4682,.T.);
#6707=EDGE_CURVE('',#5478,#5478,#4683,.T.);
#6708=EDGE_CURVE('',#5478,#5479,#3207,.T.);
#6709=EDGE_CURVE('',#5479,#5479,#4684,.T.);
#6710=EDGE_CURVE('',#5480,#5480,#4685,.T.);
#6711=EDGE_CURVE('',#5480,#5474,#3208,.T.);
#6712=EDGE_CURVE('',#5481,#5481,#4686,.T.);
#6713=EDGE_CURVE('',#5481,#5482,#3209,.T.);
#6714=EDGE_CURVE('',#5482,#5482,#4687,.T.);
#6715=EDGE_CURVE('',#5483,#5483,#4688,.T.);
#6716=EDGE_CURVE('',#5483,#5484,#3210,.T.);
#6717=EDGE_CURVE('',#5484,#5484,#4689,.T.);
#6718=EDGE_CURVE('',#5485,#5485,#4690,.T.);
#6719=EDGE_CURVE('',#5485,#5486,#3211,.T.);
#6720=EDGE_CURVE('',#5486,#5486,#4691,.T.);
#6721=EDGE_CURVE('',#5487,#5487,#4692,.T.);
#6722=EDGE_CURVE('',#5487,#5488,#3212,.T.);
#6723=EDGE_CURVE('',#5488,#5488,#4693,.T.);
#6724=EDGE_CURVE('',#5489,#5489,#4694,.T.);
#6725=EDGE_CURVE('',#5489,#5490,#3213,.T.);
#6726=EDGE_CURVE('',#5490,#5490,#4695,.T.);
#6727=EDGE_CURVE('',#5491,#5491,#4696,.T.);
#6728=EDGE_CURVE('',#5491,#5492,#3214,.T.);
#6729=EDGE_CURVE('',#5492,#5492,#4697,.T.);
#6730=EDGE_CURVE('',#5493,#5493,#4698,.T.);
#6731=EDGE_CURVE('',#5493,#5494,#3215,.T.);
#6732=EDGE_CURVE('',#5494,#5494,#4699,.T.);
#6733=EDGE_CURVE('',#5495,#5495,#4700,.T.);
#6734=EDGE_CURVE('',#5495,#5496,#3216,.T.);
#6735=EDGE_CURVE('',#5496,#5496,#4701,.T.);
#6736=EDGE_CURVE('',#5497,#5497,#4702,.T.);
#6737=EDGE_CURVE('',#5497,#5498,#3217,.T.);
#6738=EDGE_CURVE('',#5498,#5498,#4703,.T.);
#6739=EDGE_CURVE('',#5499,#5499,#4704,.T.);
#6740=EDGE_CURVE('',#5499,#5500,#3218,.T.);
#6741=EDGE_CURVE('',#5500,#5500,#4705,.T.);
#6742=EDGE_CURVE('',#5501,#5501,#4706,.T.);
#6743=EDGE_CURVE('',#5502,#5502,#4707,.T.);
#6744=EDGE_CURVE('',#5503,#5503,#4708,.T.);
#6745=EDGE_CURVE('',#5504,#5504,#4709,.T.);
#6746=EDGE_CURVE('',#5501,#5503,#3219,.T.);
#6747=EDGE_CURVE('',#5504,#5505,#3220,.T.);
#6748=EDGE_CURVE('',#5505,#5505,#4710,.T.);
#6749=EDGE_CURVE('',#5506,#5506,#4711,.T.);
#6750=EDGE_CURVE('',#5506,#5507,#3221,.T.);
#6751=EDGE_CURVE('',#5507,#5507,#4712,.T.);
#6752=EDGE_CURVE('',#5508,#5508,#4713,.T.);
#6753=EDGE_CURVE('',#5508,#5502,#3222,.T.);
#6754=EDGE_CURVE('',#5509,#5509,#4714,.T.);
#6755=EDGE_CURVE('',#5509,#5510,#3223,.T.);
#6756=EDGE_CURVE('',#5510,#5510,#4715,.T.);
#6757=EDGE_CURVE('',#5511,#5511,#4716,.T.);
#6758=EDGE_CURVE('',#5511,#5512,#3224,.T.);
#6759=EDGE_CURVE('',#5512,#5512,#4717,.T.);
#6760=EDGE_CURVE('',#5513,#5513,#4718,.T.);
#6761=EDGE_CURVE('',#5513,#5514,#3225,.T.);
#6762=EDGE_CURVE('',#5514,#5514,#4719,.T.);
#6763=EDGE_CURVE('',#5515,#5515,#4720,.T.);
#6764=EDGE_CURVE('',#5515,#5516,#3226,.T.);
#6765=EDGE_CURVE('',#5516,#5516,#4721,.T.);
#6766=EDGE_CURVE('',#5517,#5517,#4722,.T.);
#6767=EDGE_CURVE('',#5517,#5518,#3227,.T.);
#6768=EDGE_CURVE('',#5518,#5518,#4723,.T.);
#6769=EDGE_CURVE('',#5519,#5519,#4724,.T.);
#6770=EDGE_CURVE('',#5519,#5520,#3228,.T.);
#6771=EDGE_CURVE('',#5520,#5520,#4725,.T.);
#6772=EDGE_CURVE('',#5521,#5521,#4726,.T.);
#6773=EDGE_CURVE('',#5521,#5522,#3229,.T.);
#6774=EDGE_CURVE('',#5522,#5522,#4727,.T.);
#6775=EDGE_CURVE('',#5523,#5523,#4728,.T.);
#6776=EDGE_CURVE('',#5523,#5524,#3230,.T.);
#6777=EDGE_CURVE('',#5524,#5524,#4729,.T.);
#6778=EDGE_CURVE('',#5525,#5525,#4730,.T.);
#6779=EDGE_CURVE('',#5525,#5526,#3231,.T.);
#6780=EDGE_CURVE('',#5526,#5526,#4731,.T.);
#6781=EDGE_CURVE('',#5527,#5528,#459,.T.);
#6782=EDGE_CURVE('',#5529,#5527,#460,.T.);
#6783=EDGE_CURVE('',#5528,#5529,#461,.T.);
#6784=EDGE_CURVE('',#5528,#5530,#3232,.T.);
#6785=EDGE_CURVE('',#5531,#5530,#462,.T.);
#6786=EDGE_CURVE('',#5532,#5531,#463,.T.);
#6787=EDGE_CURVE('',#5533,#5532,#464,.T.);
#6788=EDGE_CURVE('',#5530,#5533,#465,.T.);
#6789=EDGE_CURVE('',#5534,#5535,#466,.T.);
#6790=EDGE_CURVE('',#5535,#5534,#467,.T.);
#6791=EDGE_CURVE('',#5535,#5536,#3233,.T.);
#6792=EDGE_CURVE('',#5537,#5536,#468,.T.);
#6793=EDGE_CURVE('',#5538,#5537,#469,.T.);
#6794=EDGE_CURVE('',#5536,#5538,#470,.T.);
#6795=EDGE_CURVE('',#5539,#5539,#4732,.T.);
#6796=EDGE_CURVE('',#5539,#5529,#3234,.T.);
#6797=EDGE_CURVE('',#5527,#5540,#3235,.T.);
#6798=EDGE_CURVE('',#5540,#5540,#4733,.T.);
#6799=EDGE_CURVE('',#5541,#5542,#471,.T.);
#6800=EDGE_CURVE('',#5542,#5543,#472,.T.);
#6801=EDGE_CURVE('',#5543,#5541,#473,.T.);
#6802=EDGE_CURVE('',#5544,#5545,#474,.T.);
#6803=EDGE_CURVE('',#5545,#5546,#475,.T.);
#6804=EDGE_CURVE('',#5546,#5544,#476,.T.);
#6805=EDGE_CURVE('',#5543,#5547,#3236,.T.);
#6806=EDGE_CURVE('',#5548,#5547,#477,.T.);
#6807=EDGE_CURVE('',#5547,#5548,#478,.T.);
#6808=EDGE_CURVE('',#5549,#5550,#479,.T.);
#6809=EDGE_CURVE('',#5550,#5549,#480,.T.);
#6810=EDGE_CURVE('',#5550,#5546,#3237,.T.);
#6811=EDGE_CURVE('',#5551,#5551,#4734,.T.);
#6812=EDGE_CURVE('',#5551,#5531,#3238,.T.);
#6813=EDGE_CURVE('',#5533,#5552,#3239,.T.);
#6814=EDGE_CURVE('',#5552,#5552,#4735,.T.);
#6815=EDGE_CURVE('',#5553,#5553,#4736,.T.);
#6816=EDGE_CURVE('',#5554,#5555,#4737,.T.);
#6817=EDGE_CURVE('',#5556,#5555,#4738,.T.);
#6818=EDGE_CURVE('',#5556,#5557,#4739,.T.);
#6819=EDGE_CURVE('',#5558,#5557,#4740,.T.);
#6820=EDGE_CURVE('',#5558,#5559,#4741,.T.);
#6821=EDGE_CURVE('',#5560,#5559,#4742,.T.);
#6822=EDGE_CURVE('',#5560,#5561,#4743,.T.);
#6823=EDGE_CURVE('',#5562,#5561,#4744,.T.);
#6824=EDGE_CURVE('',#5562,#5563,#4745,.T.);
#6825=EDGE_CURVE('',#5564,#5563,#4746,.T.);
#6826=EDGE_CURVE('',#5564,#5565,#4747,.T.);
#6827=EDGE_CURVE('',#5566,#5565,#4748,.T.);
#6828=EDGE_CURVE('',#5566,#5567,#4749,.T.);
#6829=EDGE_CURVE('',#5568,#5567,#4750,.T.);
#6830=EDGE_CURVE('',#5568,#5569,#4751,.T.);
#6831=EDGE_CURVE('',#5570,#5569,#4752,.T.);
#6832=EDGE_CURVE('',#5570,#5571,#4753,.T.);
#6833=EDGE_CURVE('',#5572,#5571,#4754,.T.);
#6834=EDGE_CURVE('',#5572,#5573,#4755,.T.);
#6835=EDGE_CURVE('',#5574,#5573,#4756,.T.);
#6836=EDGE_CURVE('',#5574,#5575,#4757,.T.);
#6837=EDGE_CURVE('',#5576,#5575,#4758,.T.);
#6838=EDGE_CURVE('',#5576,#5577,#4759,.T.);
#6839=EDGE_CURVE('',#5578,#5577,#4760,.T.);
#6840=EDGE_CURVE('',#5578,#5579,#4761,.T.);
#6841=EDGE_CURVE('',#5580,#5579,#4762,.T.);
#6842=EDGE_CURVE('',#5580,#5581,#4763,.T.);
#6843=EDGE_CURVE('',#5582,#5581,#4764,.T.);
#6844=EDGE_CURVE('',#5582,#5583,#4765,.T.);
#6845=EDGE_CURVE('',#5584,#5583,#4766,.T.);
#6846=EDGE_CURVE('',#5584,#5585,#4767,.T.);
#6847=EDGE_CURVE('',#5586,#5585,#4768,.T.);
#6848=EDGE_CURVE('',#5586,#5587,#4769,.T.);
#6849=EDGE_CURVE('',#5588,#5587,#4770,.T.);
#6850=EDGE_CURVE('',#5588,#5589,#4771,.T.);
#6851=EDGE_CURVE('',#5590,#5589,#4772,.T.);
#6852=EDGE_CURVE('',#5590,#5591,#4773,.T.);
#6853=EDGE_CURVE('',#5592,#5591,#4774,.T.);
#6854=EDGE_CURVE('',#5592,#5593,#4775,.T.);
#6855=EDGE_CURVE('',#5554,#5593,#4776,.T.);
#6856=EDGE_CURVE('',#5594,#5594,#4777,.T.);
#6857=EDGE_CURVE('',#5594,#5553,#3240,.T.);
#6858=EDGE_CURVE('',#5595,#5595,#4778,.T.);
#6859=EDGE_CURVE('',#5596,#5597,#4779,.T.);
#6860=EDGE_CURVE('',#5597,#5598,#4780,.T.);
#6861=EDGE_CURVE('',#5598,#5599,#4781,.T.);
#6862=EDGE_CURVE('',#5599,#5600,#4782,.T.);
#6863=EDGE_CURVE('',#5600,#5601,#4783,.T.);
#6864=EDGE_CURVE('',#5601,#5602,#4784,.T.);
#6865=EDGE_CURVE('',#5602,#5603,#4785,.T.);
#6866=EDGE_CURVE('',#5603,#5604,#4786,.T.);
#6867=EDGE_CURVE('',#5604,#5605,#4787,.T.);
#6868=EDGE_CURVE('',#5605,#5606,#4788,.T.);
#6869=EDGE_CURVE('',#5606,#5607,#4789,.T.);
#6870=EDGE_CURVE('',#5607,#5608,#4790,.T.);
#6871=EDGE_CURVE('',#5608,#5609,#4791,.T.);
#6872=EDGE_CURVE('',#5609,#5610,#4792,.T.);
#6873=EDGE_CURVE('',#5610,#5611,#4793,.T.);
#6874=EDGE_CURVE('',#5611,#5612,#4794,.T.);
#6875=EDGE_CURVE('',#5612,#5613,#4795,.T.);
#6876=EDGE_CURVE('',#5613,#5614,#4796,.T.);
#6877=EDGE_CURVE('',#5614,#5615,#4797,.T.);
#6878=EDGE_CURVE('',#5615,#5616,#4798,.T.);
#6879=EDGE_CURVE('',#5616,#5617,#4799,.T.);
#6880=EDGE_CURVE('',#5617,#5618,#4800,.T.);
#6881=EDGE_CURVE('',#5618,#5619,#4801,.T.);
#6882=EDGE_CURVE('',#5619,#5620,#4802,.T.);
#6883=EDGE_CURVE('',#5620,#5621,#4803,.T.);
#6884=EDGE_CURVE('',#5621,#5622,#4804,.T.);
#6885=EDGE_CURVE('',#5622,#5623,#4805,.T.);
#6886=EDGE_CURVE('',#5623,#5624,#4806,.T.);
#6887=EDGE_CURVE('',#5624,#5625,#4807,.T.);
#6888=EDGE_CURVE('',#5625,#5626,#4808,.T.);
#6889=EDGE_CURVE('',#5626,#5627,#4809,.T.);
#6890=EDGE_CURVE('',#5627,#5628,#4810,.T.);
#6891=EDGE_CURVE('',#5628,#5629,#4811,.T.);
#6892=EDGE_CURVE('',#5629,#5630,#4812,.T.);
#6893=EDGE_CURVE('',#5630,#5631,#4813,.T.);
#6894=EDGE_CURVE('',#5631,#5632,#4814,.T.);
#6895=EDGE_CURVE('',#5632,#5633,#4815,.T.);
#6896=EDGE_CURVE('',#5633,#5634,#4816,.T.);
#6897=EDGE_CURVE('',#5634,#5635,#4817,.T.);
#6898=EDGE_CURVE('',#5635,#5596,#4818,.T.);
#6899=EDGE_CURVE('',#5636,#5636,#4819,.T.);
#6900=EDGE_CURVE('',#5636,#5595,#3241,.T.);
#6901=EDGE_CURVE('',#5597,#5554,#3242,.T.);
#6902=EDGE_CURVE('',#5555,#5596,#3243,.T.);
#6903=EDGE_CURVE('',#5635,#5556,#3244,.T.);
#6904=EDGE_CURVE('',#5557,#5634,#3245,.T.);
#6905=EDGE_CURVE('',#5633,#5558,#3246,.T.);
#6906=EDGE_CURVE('',#5559,#5632,#3247,.T.);
#6907=EDGE_CURVE('',#5631,#5560,#3248,.T.);
#6908=EDGE_CURVE('',#5561,#5630,#3249,.T.);
#6909=EDGE_CURVE('',#5629,#5562,#3250,.T.);
#6910=EDGE_CURVE('',#5563,#5628,#3251,.T.);
#6911=EDGE_CURVE('',#5627,#5564,#3252,.T.);
#6912=EDGE_CURVE('',#5565,#5626,#3253,.T.);
#6913=EDGE_CURVE('',#5625,#5566,#3254,.T.);
#6914=EDGE_CURVE('',#5567,#5624,#3255,.T.);
#6915=EDGE_CURVE('',#5623,#5568,#3256,.T.);
#6916=EDGE_CURVE('',#5569,#5622,#3257,.T.);
#6917=EDGE_CURVE('',#5621,#5570,#3258,.T.);
#6918=EDGE_CURVE('',#5571,#5620,#3259,.T.);
#6919=EDGE_CURVE('',#5619,#5572,#3260,.T.);
#6920=EDGE_CURVE('',#5573,#5618,#3261,.T.);
#6921=EDGE_CURVE('',#5617,#5574,#3262,.T.);
#6922=EDGE_CURVE('',#5575,#5616,#3263,.T.);
#6923=EDGE_CURVE('',#5615,#5576,#3264,.T.);
#6924=EDGE_CURVE('',#5577,#5614,#3265,.T.);
#6925=EDGE_CURVE('',#5613,#5578,#3266,.T.);
#6926=EDGE_CURVE('',#5579,#5612,#3267,.T.);
#6927=EDGE_CURVE('',#5611,#5580,#3268,.T.);
#6928=EDGE_CURVE('',#5581,#5610,#3269,.T.);
#6929=EDGE_CURVE('',#5609,#5582,#3270,.T.);
#6930=EDGE_CURVE('',#5583,#5608,#3271,.T.);
#6931=EDGE_CURVE('',#5607,#5584,#3272,.T.);
#6932=EDGE_CURVE('',#5585,#5606,#3273,.T.);
#6933=EDGE_CURVE('',#5605,#5586,#3274,.T.);
#6934=EDGE_CURVE('',#5587,#5604,#3275,.T.);
#6935=EDGE_CURVE('',#5603,#5588,#3276,.T.);
#6936=EDGE_CURVE('',#5589,#5602,#3277,.T.);
#6937=EDGE_CURVE('',#5601,#5590,#3278,.T.);
#6938=EDGE_CURVE('',#5591,#5600,#3279,.T.);
#6939=EDGE_CURVE('',#5593,#5598,#3280,.T.);
#6940=EDGE_CURVE('',#5599,#5592,#3281,.T.);
#6941=EDGE_CURVE('',#5637,#5637,#4820,.T.);
#6942=EDGE_CURVE('',#5637,#5638,#3282,.T.);
#6943=EDGE_CURVE('',#5638,#5638,#4821,.T.);
#6944=EDGE_CURVE('',#5639,#5639,#4822,.T.);
#6945=EDGE_CURVE('',#5640,#5640,#4823,.T.);
#6946=EDGE_CURVE('',#5640,#5641,#3283,.T.);
#6947=EDGE_CURVE('',#5641,#5641,#4824,.T.);
#6948=EDGE_CURVE('',#5642,#5642,#4825,.T.);
#6949=EDGE_CURVE('',#5639,#5643,#3284,.T.);
#6950=EDGE_CURVE('',#5643,#5643,#4826,.T.);
#6951=EDGE_CURVE('',#5642,#5644,#3285,.T.);
#6952=EDGE_CURVE('',#5644,#5644,#4827,.T.);
#6953=EDGE_CURVE('',#5645,#5645,#4828,.T.);
#6954=EDGE_CURVE('',#5645,#5646,#3286,.T.);
#6955=EDGE_CURVE('',#5646,#5646,#4829,.T.);
#6956=EDGE_CURVE('',#5647,#5647,#4830,.T.);
#6957=EDGE_CURVE('',#5647,#5648,#3287,.T.);
#6958=EDGE_CURVE('',#5648,#5648,#4831,.T.);
#6959=EDGE_CURVE('',#5649,#5649,#4832,.T.);
#6960=EDGE_CURVE('',#5649,#5650,#3288,.T.);
#6961=EDGE_CURVE('',#5650,#5650,#4833,.T.);
#6962=EDGE_CURVE('',#5651,#5651,#4834,.T.);
#6963=EDGE_CURVE('',#5651,#5652,#3289,.T.);
#6964=EDGE_CURVE('',#5652,#5652,#4835,.T.);
#6965=EDGE_CURVE('',#5653,#5654,#3290,.T.);
#6966=EDGE_CURVE('',#5654,#5655,#3291,.T.);
#6967=EDGE_CURVE('',#5656,#5655,#3292,.T.);
#6968=EDGE_CURVE('',#5653,#5656,#3293,.T.);
#6969=EDGE_CURVE('',#5657,#5653,#3294,.T.);
#6970=EDGE_CURVE('',#5658,#5656,#3295,.T.);
#6971=EDGE_CURVE('',#5657,#5658,#3296,.T.);
#6972=EDGE_CURVE('',#5659,#5657,#3297,.T.);
#6973=EDGE_CURVE('',#5660,#5658,#3298,.T.);
#6974=EDGE_CURVE('',#5659,#5660,#3299,.T.);
#6975=EDGE_CURVE('',#5654,#5659,#3300,.T.);
#6976=EDGE_CURVE('',#5655,#5660,#3301,.T.);
#6977=EDGE_CURVE('',#5661,#5661,#4836,.T.);
#6978=EDGE_CURVE('',#5661,#5662,#3302,.T.);
#6979=EDGE_CURVE('',#5662,#5662,#4837,.T.);
#6980=EDGE_CURVE('',#5663,#5663,#4838,.T.);
#6981=EDGE_CURVE('',#5663,#5664,#3303,.T.);
#6982=EDGE_CURVE('',#5664,#5664,#4839,.T.);
#6983=EDGE_CURVE('',#5665,#5666,#3304,.T.);
#6984=EDGE_CURVE('',#5667,#5665,#4840,.T.);
#6985=EDGE_CURVE('',#5668,#5667,#3305,.T.);
#6986=EDGE_CURVE('',#5666,#5668,#3306,.T.);
#6987=EDGE_CURVE('',#5669,#5665,#3307,.T.);
#6988=EDGE_CURVE('',#5670,#5669,#4841,.T.);
#6989=EDGE_CURVE('',#5667,#5670,#3308,.T.);
#6990=EDGE_CURVE('',#5671,#5672,#3309,.T.);
#6991=EDGE_CURVE('',#5671,#5673,#4842,.T.);
#6992=EDGE_CURVE('',#5674,#5673,#3310,.T.);
#6993=EDGE_CURVE('',#5672,#5674,#4843,.T.);
#6994=EDGE_CURVE('',#5675,#5671,#3311,.T.);
#6995=EDGE_CURVE('',#5676,#5675,#3312,.T.);
#6996=EDGE_CURVE('',#5673,#5676,#3313,.T.);
#6997=EDGE_CURVE('',#5668,#5677,#3314,.T.);
#6998=EDGE_CURVE('',#5677,#5678,#3315,.T.);
#6999=EDGE_CURVE('',#5678,#5679,#3316,.T.);
#7000=EDGE_CURVE('',#5680,#5679,#3317,.T.);
#7001=EDGE_CURVE('',#5666,#5680,#3318,.T.);
#7002=EDGE_CURVE('',#5670,#5674,#3319,.T.);
#7003=EDGE_CURVE('',#5676,#5681,#3320,.T.);
#7004=EDGE_CURVE('',#5677,#5681,#3321,.T.);
#7005=EDGE_CURVE('',#5682,#5682,#4844,.T.);
#7006=EDGE_CURVE('',#5682,#5683,#3322,.T.);
#7007=EDGE_CURVE('',#5683,#5683,#4845,.T.);
#7008=EDGE_CURVE('',#5684,#5684,#4846,.T.);
#7009=EDGE_CURVE('',#5684,#5685,#3323,.T.);
#7010=EDGE_CURVE('',#5685,#5685,#4847,.T.);
#7011=EDGE_CURVE('',#5679,#5686,#3324,.T.);
#7012=EDGE_CURVE('',#5686,#5687,#3325,.T.);
#7013=EDGE_CURVE('',#5687,#5680,#3326,.T.);
#7014=EDGE_CURVE('',#5678,#5688,#3327,.T.);
#7015=EDGE_CURVE('',#5688,#5686,#3328,.T.);
#7016=EDGE_CURVE('',#5688,#5681,#3329,.T.);
#7017=EDGE_CURVE('',#5675,#5687,#3330,.T.);
#7018=EDGE_CURVE('',#5672,#5669,#3331,.T.);
#7019=EDGE_CURVE('',#5689,#5690,#3332,.T.);
#7020=EDGE_CURVE('',#5690,#5691,#3333,.T.);
#7021=EDGE_CURVE('',#5692,#5691,#3334,.T.);
#7022=EDGE_CURVE('',#5689,#5692,#3335,.T.);
#7023=EDGE_CURVE('',#5693,#5689,#3336,.T.);
#7024=EDGE_CURVE('',#5694,#5692,#3337,.T.);
#7025=EDGE_CURVE('',#5693,#5694,#3338,.T.);
#7026=EDGE_CURVE('',#5695,#5693,#3339,.T.);
#7027=EDGE_CURVE('',#5696,#5694,#3340,.T.);
#7028=EDGE_CURVE('',#5695,#5696,#3341,.T.);
#7029=EDGE_CURVE('',#5690,#5695,#3342,.T.);
#7030=EDGE_CURVE('',#5691,#5696,#3343,.T.);
#7031=EDGE_CURVE('',#5697,#5698,#3344,.T.);
#7032=EDGE_CURVE('',#5697,#5698,#4848,.T.);
#7033=EDGE_CURVE('',#5699,#5697,#3345,.T.);
#7034=EDGE_CURVE('',#5700,#5699,#4849,.T.);
#7035=EDGE_CURVE('',#5700,#5701,#3346,.T.);
#7036=EDGE_CURVE('',#5701,#5701,#4850,.T.);
#7037=EDGE_CURVE('',#5702,#5700,#4851,.T.);
#7038=EDGE_CURVE('',#5698,#5702,#3347,.T.);
#7039=EDGE_CURVE('',#5703,#5704,#3348,.T.);
#7040=EDGE_CURVE('',#5703,#5704,#4852,.T.);
#7041=EDGE_CURVE('',#5705,#5703,#3349,.T.);
#7042=EDGE_CURVE('',#5706,#5705,#4853,.T.);
#7043=EDGE_CURVE('',#5706,#5707,#3350,.T.);
#7044=EDGE_CURVE('',#5707,#5707,#4854,.T.);
#7045=EDGE_CURVE('',#5708,#5706,#4855,.T.);
#7046=EDGE_CURVE('',#5704,#5708,#3351,.T.);
#7047=EDGE_CURVE('',#5709,#5710,#3352,.T.);
#7048=EDGE_CURVE('',#5709,#5710,#4856,.T.);
#7049=EDGE_CURVE('',#5711,#5709,#3353,.T.);
#7050=EDGE_CURVE('',#5712,#5711,#4857,.T.);
#7051=EDGE_CURVE('',#5712,#5713,#3354,.T.);
#7052=EDGE_CURVE('',#5713,#5713,#4858,.T.);
#7053=EDGE_CURVE('',#5714,#5712,#4859,.T.);
#7054=EDGE_CURVE('',#5710,#5714,#3355,.T.);
#7055=EDGE_CURVE('',#5715,#5716,#3356,.T.);
#7056=EDGE_CURVE('',#5715,#5716,#4860,.T.);
#7057=EDGE_CURVE('',#5717,#5715,#3357,.T.);
#7058=EDGE_CURVE('',#5718,#5717,#4861,.T.);
#7059=EDGE_CURVE('',#5718,#5719,#3358,.T.);
#7060=EDGE_CURVE('',#5719,#5719,#4862,.T.);
#7061=EDGE_CURVE('',#5720,#5718,#4863,.T.);
#7062=EDGE_CURVE('',#5716,#5720,#3359,.T.);
#7063=EDGE_CURVE('',#5702,#5711,#3360,.T.);
#7064=EDGE_CURVE('',#5714,#5721,#3361,.T.);
#7065=EDGE_CURVE('',#5722,#5721,#3362,.T.);
#7066=EDGE_CURVE('',#5722,#5723,#3363,.T.);
#7067=EDGE_CURVE('',#5724,#5723,#3364,.T.);
#7068=EDGE_CURVE('',#5724,#5699,#3365,.T.);
#7069=EDGE_CURVE('',#5708,#5717,#3366,.T.);
#7070=EDGE_CURVE('',#5720,#5725,#3367,.T.);
#7071=EDGE_CURVE('',#5726,#5725,#3368,.T.);
#7072=EDGE_CURVE('',#5727,#5726,#3369,.T.);
#7073=EDGE_CURVE('',#5728,#5727,#3370,.T.);
#7074=EDGE_CURVE('',#5728,#5705,#3371,.T.);
#7075=EDGE_CURVE('',#5721,#5729,#3372,.T.);
#7076=EDGE_CURVE('',#5729,#5730,#3373,.T.);
#7077=EDGE_CURVE('',#5730,#5731,#3374,.T.);
#7078=EDGE_CURVE('',#5731,#5732,#3375,.T.);
#7079=EDGE_CURVE('',#5732,#5728,#3376,.T.);
#7080=EDGE_CURVE('',#5727,#5733,#3377,.T.);
#7081=EDGE_CURVE('',#5733,#5734,#3378,.T.);
#7082=EDGE_CURVE('',#5734,#5735,#3379,.T.);
#7083=EDGE_CURVE('',#5735,#5736,#3380,.T.);
#7084=EDGE_CURVE('',#5736,#5722,#3381,.T.);
#7085=EDGE_CURVE('',#5737,#5724,#3382,.T.);
#7086=EDGE_CURVE('',#5729,#5737,#3383,.T.);
#7087=EDGE_CURVE('',#5738,#5737,#3384,.T.);
#7088=EDGE_CURVE('',#5730,#5738,#3385,.T.);
#7089=EDGE_CURVE('',#5739,#5738,#3386,.T.);
#7090=EDGE_CURVE('',#5731,#5739,#3387,.T.);
#7091=EDGE_CURVE('',#5740,#5739,#3388,.T.);
#7092=EDGE_CURVE('',#5732,#5740,#3389,.T.);
#7093=EDGE_CURVE('',#5725,#5740,#3390,.T.);
#7094=EDGE_CURVE('',#5741,#5726,#3391,.T.);
#7095=EDGE_CURVE('',#5733,#5741,#3392,.T.);
#7096=EDGE_CURVE('',#5742,#5741,#3393,.T.);
#7097=EDGE_CURVE('',#5734,#5742,#3394,.T.);
#7098=EDGE_CURVE('',#5743,#5742,#3395,.T.);
#7099=EDGE_CURVE('',#5735,#5743,#3396,.T.);
#7100=EDGE_CURVE('',#5744,#5743,#3397,.T.);
#7101=EDGE_CURVE('',#5736,#5744,#3398,.T.);
#7102=EDGE_CURVE('',#5723,#5744,#3399,.T.);
#7103=EDGE_CURVE('',#5745,#5746,#3400,.T.);
#7104=EDGE_CURVE('',#5746,#5747,#3401,.T.);
#7105=EDGE_CURVE('',#5748,#5747,#3402,.T.);
#7106=EDGE_CURVE('',#5745,#5748,#3403,.T.);
#7107=EDGE_CURVE('',#5749,#5745,#3404,.T.);
#7108=EDGE_CURVE('',#5750,#5748,#3405,.T.);
#7109=EDGE_CURVE('',#5749,#5750,#3406,.T.);
#7110=EDGE_CURVE('',#5751,#5749,#3407,.T.);
#7111=EDGE_CURVE('',#5752,#5750,#3408,.T.);
#7112=EDGE_CURVE('',#5751,#5752,#3409,.T.);
#7113=EDGE_CURVE('',#5753,#5751,#3410,.T.);
#7114=EDGE_CURVE('',#5754,#5752,#3411,.T.);
#7115=EDGE_CURVE('',#5753,#5754,#3412,.T.);
#7116=EDGE_CURVE('',#5755,#5753,#3413,.T.);
#7117=EDGE_CURVE('',#5756,#5754,#3414,.T.);
#7118=EDGE_CURVE('',#5755,#5756,#3415,.T.);
#7119=EDGE_CURVE('',#5757,#5755,#3416,.T.);
#7120=EDGE_CURVE('',#5758,#5756,#3417,.T.);
#7121=EDGE_CURVE('',#5757,#5758,#3418,.T.);
#7122=EDGE_CURVE('',#5759,#5757,#3419,.T.);
#7123=EDGE_CURVE('',#5760,#5758,#3420,.T.);
#7124=EDGE_CURVE('',#5759,#5760,#3421,.T.);
#7125=EDGE_CURVE('',#5746,#5759,#3422,.T.);
#7126=EDGE_CURVE('',#5747,#5760,#3423,.T.);
#7127=EDGE_CURVE('',#5761,#5762,#3424,.T.);
#7128=EDGE_CURVE('',#5761,#5763,#3425,.T.);
#7129=EDGE_CURVE('',#5764,#5763,#3426,.T.);
#7130=EDGE_CURVE('',#5762,#5764,#3427,.T.);
#7131=EDGE_CURVE('',#5762,#5765,#3428,.T.);
#7132=EDGE_CURVE('',#5766,#5764,#3429,.T.);
#7133=EDGE_CURVE('',#5765,#5766,#3430,.T.);
#7134=EDGE_CURVE('',#5765,#5767,#3431,.T.);
#7135=EDGE_CURVE('',#5768,#5766,#3432,.T.);
#7136=EDGE_CURVE('',#5767,#5768,#3433,.T.);
#7137=EDGE_CURVE('',#5767,#5769,#3434,.T.);
#7138=EDGE_CURVE('',#5770,#5768,#3435,.T.);
#7139=EDGE_CURVE('',#5769,#5770,#3436,.T.);
#7140=EDGE_CURVE('',#5769,#5771,#3437,.T.);
#7141=EDGE_CURVE('',#5772,#5770,#3438,.T.);
#7142=EDGE_CURVE('',#5771,#5772,#3439,.T.);
#7143=EDGE_CURVE('',#5771,#5773,#3440,.T.);
#7144=EDGE_CURVE('',#5774,#5772,#3441,.T.);
#7145=EDGE_CURVE('',#5773,#5774,#3442,.T.);
#7146=EDGE_CURVE('',#5773,#5775,#3443,.T.);
#7147=EDGE_CURVE('',#5776,#5774,#3444,.T.);
#7148=EDGE_CURVE('',#5775,#5776,#3445,.T.);
#7149=EDGE_CURVE('',#5775,#5761,#3446,.T.);
#7150=EDGE_CURVE('',#5763,#5776,#3447,.T.);
#7151=EDGE_CURVE('',#5777,#5777,#4864,.T.);
#7152=EDGE_CURVE('',#5777,#5778,#3448,.T.);
#7153=EDGE_CURVE('',#5778,#5778,#4865,.T.);
#7154=EDGE_CURVE('',#5778,#5779,#3449,.T.);
#7155=EDGE_CURVE('',#5779,#5779,#4866,.T.);
#7156=EDGE_CURVE('',#5780,#5780,#4867,.T.);
#7157=EDGE_CURVE('',#5780,#5781,#3450,.T.);
#7158=EDGE_CURVE('',#5781,#5781,#4868,.T.);
#7159=EDGE_CURVE('',#5782,#5782,#4869,.T.);
#7160=EDGE_CURVE('',#5783,#5783,#4870,.T.);
#7161=EDGE_CURVE('',#5783,#5782,#3451,.T.);
#7162=EDGE_CURVE('',#5784,#5784,#4871,.T.);
#7163=EDGE_CURVE('',#5784,#5783,#3452,.T.);
#7164=EDGE_CURVE('',#5785,#5785,#4872,.T.);
#7165=EDGE_CURVE('',#5785,#5784,#3453,.T.);
#7166=EDGE_CURVE('',#5786,#5786,#4873,.T.);
#7167=EDGE_CURVE('',#5787,#5787,#4874,.F.);
#7168=EDGE_CURVE('',#5787,#5786,#3454,.T.);
#7169=EDGE_CURVE('',#5788,#5788,#4875,.F.);
#7170=EDGE_CURVE('',#5788,#5787,#3455,.T.);
#7171=EDGE_CURVE('',#5789,#5789,#4876,.T.);
#7172=EDGE_CURVE('',#5789,#5788,#3456,.T.);
#7173=EDGE_CURVE('',#5790,#5791,#3457,.T.);
#7174=EDGE_CURVE('',#5791,#5792,#3458,.T.);
#7175=EDGE_CURVE('',#5792,#5793,#3459,.T.);
#7176=EDGE_CURVE('',#5790,#5793,#3460,.T.);
#7177=EDGE_CURVE('',#5791,#5794,#3461,.T.);
#7178=EDGE_CURVE('',#5794,#5795,#3462,.T.);
#7179=EDGE_CURVE('',#5795,#5792,#3463,.T.);
#7180=EDGE_CURVE('',#5794,#5796,#3464,.T.);
#7181=EDGE_CURVE('',#5796,#5797,#3465,.T.);
#7182=EDGE_CURVE('',#5797,#5795,#3466,.T.);
#7183=EDGE_CURVE('',#5796,#5798,#3467,.T.);
#7184=EDGE_CURVE('',#5798,#5799,#3468,.T.);
#7185=EDGE_CURVE('',#5799,#5797,#3469,.T.);
#7186=EDGE_CURVE('',#5798,#5800,#3470,.T.);
#7187=EDGE_CURVE('',#5800,#5801,#3471,.T.);
#7188=EDGE_CURVE('',#5801,#5799,#3472,.T.);
#7189=EDGE_CURVE('',#5800,#5790,#3473,.T.);
#7190=EDGE_CURVE('',#5793,#5801,#3474,.T.);
#7191=EDGE_CURVE('',#5802,#5803,#3475,.T.);
#7192=EDGE_CURVE('',#5803,#5804,#3476,.T.);
#7193=EDGE_CURVE('',#5804,#5805,#3477,.T.);
#7194=EDGE_CURVE('',#5802,#5805,#3478,.T.);
#7195=EDGE_CURVE('',#5803,#5806,#3479,.T.);
#7196=EDGE_CURVE('',#5806,#5807,#3480,.T.);
#7197=EDGE_CURVE('',#5807,#5804,#3481,.T.);
#7198=EDGE_CURVE('',#5806,#5808,#3482,.T.);
#7199=EDGE_CURVE('',#5808,#5809,#3483,.T.);
#7200=EDGE_CURVE('',#5809,#5807,#3484,.T.);
#7201=EDGE_CURVE('',#5808,#5810,#3485,.T.);
#7202=EDGE_CURVE('',#5810,#5811,#3486,.T.);
#7203=EDGE_CURVE('',#5811,#5809,#3487,.T.);
#7204=EDGE_CURVE('',#5810,#5812,#3488,.T.);
#7205=EDGE_CURVE('',#5812,#5813,#3489,.T.);
#7206=EDGE_CURVE('',#5813,#5811,#3490,.T.);
#7207=EDGE_CURVE('',#5812,#5802,#3491,.T.);
#7208=EDGE_CURVE('',#5805,#5813,#3492,.T.);
#7209=EDGE_CURVE('',#5814,#5814,#4877,.T.);
#7210=EDGE_CURVE('',#5815,#5815,#4878,.T.);
#7211=EDGE_CURVE('',#5816,#5816,#4879,.T.);
#7212=EDGE_CURVE('',#5816,#5815,#3493,.T.);
#7213=EDGE_CURVE('',#5817,#5817,#4880,.T.);
#7214=EDGE_CURVE('',#5817,#5816,#3494,.T.);
#7215=EDGE_CURVE('',#5818,#5818,#4881,.T.);
#7216=EDGE_CURVE('',#5818,#5817,#3495,.T.);
#7217=EDGE_CURVE('',#5819,#5819,#4882,.T.);
#7218=EDGE_CURVE('',#5820,#5820,#4883,.F.);
#7219=EDGE_CURVE('',#5820,#5819,#3496,.T.);
#7220=EDGE_CURVE('',#5814,#5820,#3497,.T.);
#7221=EDGE_CURVE('',#5821,#5821,#4884,.T.);
#7222=EDGE_CURVE('',#5822,#5822,#4885,.T.);
#7223=EDGE_CURVE('',#5822,#5821,#3498,.T.);
#7224=EDGE_CURVE('',#5823,#5823,#4886,.T.);
#7225=EDGE_CURVE('',#5823,#5822,#3499,.T.);
#7226=EDGE_CURVE('',#5824,#5824,#4887,.T.);
#7227=EDGE_CURVE('',#5824,#5823,#3500,.T.);
#7228=EDGE_CURVE('',#5825,#5825,#4888,.T.);
#7229=EDGE_CURVE('',#5826,#5826,#4889,.F.);
#7230=EDGE_CURVE('',#5826,#5825,#3501,.T.);
#7231=EDGE_CURVE('',#5827,#5827,#4890,.F.);
#7232=EDGE_CURVE('',#5827,#5826,#3502,.T.);
#7233=EDGE_CURVE('',#5828,#5828,#4891,.T.);
#7234=EDGE_CURVE('',#5828,#5827,#3503,.T.);
#7235=EDGE_CURVE('',#5829,#5830,#3504,.T.);
#7236=EDGE_CURVE('',#5830,#5831,#3505,.T.);
#7237=EDGE_CURVE('',#5831,#5832,#3506,.T.);
#7238=EDGE_CURVE('',#5829,#5832,#3507,.T.);
#7239=EDGE_CURVE('',#5830,#5833,#3508,.T.);
#7240=EDGE_CURVE('',#5833,#5834,#3509,.T.);
#7241=EDGE_CURVE('',#5834,#5831,#3510,.T.);
#7242=EDGE_CURVE('',#5833,#5835,#3511,.T.);
#7243=EDGE_CURVE('',#5835,#5836,#3512,.T.);
#7244=EDGE_CURVE('',#5836,#5834,#3513,.T.);
#7245=EDGE_CURVE('',#5835,#5837,#3514,.T.);
#7246=EDGE_CURVE('',#5837,#5838,#3515,.T.);
#7247=EDGE_CURVE('',#5838,#5836,#3516,.T.);
#7248=EDGE_CURVE('',#5837,#5839,#3517,.T.);
#7249=EDGE_CURVE('',#5839,#5840,#3518,.T.);
#7250=EDGE_CURVE('',#5840,#5838,#3519,.T.);
#7251=EDGE_CURVE('',#5839,#5829,#3520,.T.);
#7252=EDGE_CURVE('',#5832,#5840,#3521,.T.);
#7253=ORIENTED_EDGE('',*,*,#5841,.F.);
#7254=ORIENTED_EDGE('',*,*,#5842,.T.);
#7255=ORIENTED_EDGE('',*,*,#5843,.F.);
#7256=ORIENTED_EDGE('',*,*,#5842,.F.);
#7257=ORIENTED_EDGE('',*,*,#5841,.T.);
#7258=ORIENTED_EDGE('',*,*,#5844,.F.);
#7259=ORIENTED_EDGE('',*,*,#5845,.T.);
#7260=ORIENTED_EDGE('',*,*,#5846,.F.);
#7261=ORIENTED_EDGE('',*,*,#5845,.F.);
#7262=ORIENTED_EDGE('',*,*,#5844,.T.);
#7263=ORIENTED_EDGE('',*,*,#5847,.F.);
#7264=ORIENTED_EDGE('',*,*,#5848,.T.);
#7265=ORIENTED_EDGE('',*,*,#5849,.F.);
#7266=ORIENTED_EDGE('',*,*,#5848,.F.);
#7267=ORIENTED_EDGE('',*,*,#5847,.T.);
#7268=ORIENTED_EDGE('',*,*,#5850,.F.);
#7269=ORIENTED_EDGE('',*,*,#5851,.T.);
#7270=ORIENTED_EDGE('',*,*,#5852,.F.);
#7271=ORIENTED_EDGE('',*,*,#5851,.F.);
#7272=ORIENTED_EDGE('',*,*,#5850,.T.);
#7273=ORIENTED_EDGE('',*,*,#5853,.F.);
#7274=ORIENTED_EDGE('',*,*,#5854,.T.);
#7275=ORIENTED_EDGE('',*,*,#5855,.F.);
#7276=ORIENTED_EDGE('',*,*,#5854,.F.);
#7277=ORIENTED_EDGE('',*,*,#5853,.T.);
#7278=ORIENTED_EDGE('',*,*,#5856,.F.);
#7279=ORIENTED_EDGE('',*,*,#5857,.T.);
#7280=ORIENTED_EDGE('',*,*,#5858,.F.);
#7281=ORIENTED_EDGE('',*,*,#5857,.F.);
#7282=ORIENTED_EDGE('',*,*,#5856,.T.);
#7283=ORIENTED_EDGE('',*,*,#5859,.F.);
#7284=ORIENTED_EDGE('',*,*,#5860,.T.);
#7285=ORIENTED_EDGE('',*,*,#5861,.F.);
#7286=ORIENTED_EDGE('',*,*,#5860,.F.);
#7287=ORIENTED_EDGE('',*,*,#5859,.T.);
#7288=ORIENTED_EDGE('',*,*,#5862,.F.);
#7289=ORIENTED_EDGE('',*,*,#5863,.T.);
#7290=ORIENTED_EDGE('',*,*,#5864,.F.);
#7291=ORIENTED_EDGE('',*,*,#5863,.F.);
#7292=ORIENTED_EDGE('',*,*,#5862,.T.);
#7293=ORIENTED_EDGE('',*,*,#5865,.F.);
#7294=ORIENTED_EDGE('',*,*,#5866,.T.);
#7295=ORIENTED_EDGE('',*,*,#5867,.F.);
#7296=ORIENTED_EDGE('',*,*,#5866,.F.);
#7297=ORIENTED_EDGE('',*,*,#5868,.F.);
#7298=ORIENTED_EDGE('',*,*,#5869,.T.);
#7299=ORIENTED_EDGE('',*,*,#5870,.F.);
#7300=ORIENTED_EDGE('',*,*,#5869,.F.);
#7301=ORIENTED_EDGE('',*,*,#5871,.F.);
#7302=ORIENTED_EDGE('',*,*,#5872,.T.);
#7303=ORIENTED_EDGE('',*,*,#5873,.F.);
#7304=ORIENTED_EDGE('',*,*,#5872,.F.);
#7305=ORIENTED_EDGE('',*,*,#5874,.F.);
#7306=ORIENTED_EDGE('',*,*,#5875,.T.);
#7307=ORIENTED_EDGE('',*,*,#5876,.F.);
#7308=ORIENTED_EDGE('',*,*,#5875,.F.);
#7309=ORIENTED_EDGE('',*,*,#5877,.F.);
#7310=ORIENTED_EDGE('',*,*,#5878,.T.);
#7311=ORIENTED_EDGE('',*,*,#5879,.F.);
#7312=ORIENTED_EDGE('',*,*,#5878,.F.);
#7313=ORIENTED_EDGE('',*,*,#5877,.T.);
#7314=ORIENTED_EDGE('',*,*,#5880,.F.);
#7315=ORIENTED_EDGE('',*,*,#5881,.T.);
#7316=ORIENTED_EDGE('',*,*,#5882,.F.);
#7317=ORIENTED_EDGE('',*,*,#5881,.F.);
#7318=ORIENTED_EDGE('',*,*,#5880,.T.);
#7319=ORIENTED_EDGE('',*,*,#5883,.F.);
#7320=ORIENTED_EDGE('',*,*,#5884,.T.);
#7321=ORIENTED_EDGE('',*,*,#5885,.F.);
#7322=ORIENTED_EDGE('',*,*,#5884,.F.);
#7323=ORIENTED_EDGE('',*,*,#5883,.T.);
#7324=ORIENTED_EDGE('',*,*,#5886,.F.);
#7325=ORIENTED_EDGE('',*,*,#5887,.T.);
#7326=ORIENTED_EDGE('',*,*,#5888,.F.);
#7327=ORIENTED_EDGE('',*,*,#5887,.F.);
#7328=ORIENTED_EDGE('',*,*,#5886,.T.);
#7329=ORIENTED_EDGE('',*,*,#5889,.F.);
#7330=ORIENTED_EDGE('',*,*,#5890,.T.);
#7331=ORIENTED_EDGE('',*,*,#5891,.F.);
#7332=ORIENTED_EDGE('',*,*,#5890,.F.);
#7333=ORIENTED_EDGE('',*,*,#5889,.T.);
#7334=ORIENTED_EDGE('',*,*,#5892,.F.);
#7335=ORIENTED_EDGE('',*,*,#5893,.T.);
#7336=ORIENTED_EDGE('',*,*,#5894,.F.);
#7337=ORIENTED_EDGE('',*,*,#5893,.F.);
#7338=ORIENTED_EDGE('',*,*,#5892,.T.);
#7339=ORIENTED_EDGE('',*,*,#5895,.F.);
#7340=ORIENTED_EDGE('',*,*,#5896,.T.);
#7341=ORIENTED_EDGE('',*,*,#5897,.F.);
#7342=ORIENTED_EDGE('',*,*,#5896,.F.);
#7343=ORIENTED_EDGE('',*,*,#5895,.T.);
#7344=ORIENTED_EDGE('',*,*,#5898,.F.);
#7345=ORIENTED_EDGE('',*,*,#5899,.T.);
#7346=ORIENTED_EDGE('',*,*,#5900,.F.);
#7347=ORIENTED_EDGE('',*,*,#5899,.F.);
#7348=ORIENTED_EDGE('',*,*,#5898,.T.);
#7349=ORIENTED_EDGE('',*,*,#5901,.T.);
#7350=ORIENTED_EDGE('',*,*,#5902,.T.);
#7351=ORIENTED_EDGE('',*,*,#5903,.F.);
#7352=ORIENTED_EDGE('',*,*,#5904,.F.);
#7353=ORIENTED_EDGE('',*,*,#5905,.T.);
#7354=ORIENTED_EDGE('',*,*,#5904,.T.);
#7355=ORIENTED_EDGE('',*,*,#5906,.F.);
#7356=ORIENTED_EDGE('',*,*,#5907,.F.);
#7357=ORIENTED_EDGE('',*,*,#5908,.T.);
#7358=ORIENTED_EDGE('',*,*,#5907,.T.);
#7359=ORIENTED_EDGE('',*,*,#5909,.F.);
#7360=ORIENTED_EDGE('',*,*,#5910,.F.);
#7361=ORIENTED_EDGE('',*,*,#5911,.T.);
#7362=ORIENTED_EDGE('',*,*,#5910,.T.);
#7363=ORIENTED_EDGE('',*,*,#5912,.F.);
#7364=ORIENTED_EDGE('',*,*,#5902,.F.);
#7365=ORIENTED_EDGE('',*,*,#5912,.T.);
#7366=ORIENTED_EDGE('',*,*,#5909,.T.);
#7367=ORIENTED_EDGE('',*,*,#5906,.T.);
#7368=ORIENTED_EDGE('',*,*,#5903,.T.);
#7369=ORIENTED_EDGE('',*,*,#5849,.T.);
#7370=ORIENTED_EDGE('',*,*,#5852,.T.);
#7371=ORIENTED_EDGE('',*,*,#5858,.T.);
#7372=ORIENTED_EDGE('',*,*,#5864,.T.);
#7373=ORIENTED_EDGE('',*,*,#5870,.T.);
#7374=ORIENTED_EDGE('',*,*,#5876,.T.);
#7375=ORIENTED_EDGE('',*,*,#5900,.T.);
#7376=ORIENTED_EDGE('',*,*,#5897,.T.);
#7377=ORIENTED_EDGE('',*,*,#5894,.T.);
#7378=ORIENTED_EDGE('',*,*,#5891,.T.);
#7379=ORIENTED_EDGE('',*,*,#5888,.T.);
#7380=ORIENTED_EDGE('',*,*,#5885,.T.);
#7381=ORIENTED_EDGE('',*,*,#5882,.T.);
#7382=ORIENTED_EDGE('',*,*,#5879,.T.);
#7383=ORIENTED_EDGE('',*,*,#5873,.T.);
#7384=ORIENTED_EDGE('',*,*,#5867,.T.);
#7385=ORIENTED_EDGE('',*,*,#5861,.T.);
#7386=ORIENTED_EDGE('',*,*,#5855,.T.);
#7387=ORIENTED_EDGE('',*,*,#5846,.T.);
#7388=ORIENTED_EDGE('',*,*,#5843,.T.);
#7389=ORIENTED_EDGE('',*,*,#5911,.F.);
#7390=ORIENTED_EDGE('',*,*,#5901,.F.);
#7391=ORIENTED_EDGE('',*,*,#5905,.F.);
#7392=ORIENTED_EDGE('',*,*,#5908,.F.);
#7393=ORIENTED_EDGE('',*,*,#5865,.T.);
#7394=ORIENTED_EDGE('',*,*,#5868,.T.);
#7395=ORIENTED_EDGE('',*,*,#5871,.T.);
#7396=ORIENTED_EDGE('',*,*,#5874,.T.);
#7397=ORIENTED_EDGE('',*,*,#5913,.F.);
#7398=ORIENTED_EDGE('',*,*,#5914,.F.);
#7399=ORIENTED_EDGE('',*,*,#5915,.F.);
#7400=ORIENTED_EDGE('',*,*,#5916,.F.);
#7401=ORIENTED_EDGE('',*,*,#5915,.T.);
#7402=ORIENTED_EDGE('',*,*,#5917,.T.);
#7403=ORIENTED_EDGE('',*,*,#5918,.T.);
#7404=ORIENTED_EDGE('',*,*,#5919,.T.);
#7405=ORIENTED_EDGE('',*,*,#5914,.T.);
#7406=ORIENTED_EDGE('',*,*,#5920,.T.);
#7407=ORIENTED_EDGE('',*,*,#5921,.T.);
#7408=ORIENTED_EDGE('',*,*,#5917,.F.);
#7409=ORIENTED_EDGE('',*,*,#5921,.F.);
#7410=ORIENTED_EDGE('',*,*,#5922,.F.);
#7411=ORIENTED_EDGE('',*,*,#5923,.F.);
#7412=ORIENTED_EDGE('',*,*,#5918,.F.);
#7413=ORIENTED_EDGE('',*,*,#5913,.T.);
#7414=ORIENTED_EDGE('',*,*,#5924,.F.);
#7415=ORIENTED_EDGE('',*,*,#5922,.T.);
#7416=ORIENTED_EDGE('',*,*,#5920,.F.);
#7417=ORIENTED_EDGE('',*,*,#5916,.T.);
#7418=ORIENTED_EDGE('',*,*,#5919,.F.);
#7419=ORIENTED_EDGE('',*,*,#5923,.T.);
#7420=ORIENTED_EDGE('',*,*,#5924,.T.);
#7421=ORIENTED_EDGE('',*,*,#5925,.T.);
#7422=ORIENTED_EDGE('',*,*,#5926,.T.);
#7423=ORIENTED_EDGE('',*,*,#5927,.F.);
#7424=ORIENTED_EDGE('',*,*,#5928,.F.);
#7425=ORIENTED_EDGE('',*,*,#5929,.T.);
#7426=ORIENTED_EDGE('',*,*,#5930,.T.);
#7427=ORIENTED_EDGE('',*,*,#5928,.T.);
#7428=ORIENTED_EDGE('',*,*,#5931,.F.);
#7429=ORIENTED_EDGE('',*,*,#5932,.T.);
#7430=ORIENTED_EDGE('',*,*,#5931,.T.);
#7431=ORIENTED_EDGE('',*,*,#5927,.T.);
#7432=ORIENTED_EDGE('',*,*,#5933,.T.);
#7433=ORIENTED_EDGE('',*,*,#5934,.T.);
#7434=ORIENTED_EDGE('',*,*,#5933,.F.);
#7435=ORIENTED_EDGE('',*,*,#5926,.F.);
#7436=ORIENTED_EDGE('',*,*,#5935,.T.);
#7437=ORIENTED_EDGE('',*,*,#5936,.T.);
#7438=ORIENTED_EDGE('',*,*,#5935,.F.);
#7439=ORIENTED_EDGE('',*,*,#5925,.F.);
#7440=ORIENTED_EDGE('',*,*,#5930,.F.);
#7441=ORIENTED_EDGE('',*,*,#5929,.F.);
#7442=ORIENTED_EDGE('',*,*,#5932,.F.);
#7443=ORIENTED_EDGE('',*,*,#5934,.F.);
#7444=ORIENTED_EDGE('',*,*,#5936,.F.);
#7445=ORIENTED_EDGE('',*,*,#5937,.F.);
#7446=ORIENTED_EDGE('',*,*,#5938,.F.);
#7447=ORIENTED_EDGE('',*,*,#5939,.F.);
#7448=ORIENTED_EDGE('',*,*,#5940,.F.);
#7449=ORIENTED_EDGE('',*,*,#5939,.T.);
#7450=ORIENTED_EDGE('',*,*,#5941,.T.);
#7451=ORIENTED_EDGE('',*,*,#5942,.T.);
#7452=ORIENTED_EDGE('',*,*,#5943,.T.);
#7453=ORIENTED_EDGE('',*,*,#5938,.T.);
#7454=ORIENTED_EDGE('',*,*,#5944,.T.);
#7455=ORIENTED_EDGE('',*,*,#5945,.T.);
#7456=ORIENTED_EDGE('',*,*,#5941,.F.);
#7457=ORIENTED_EDGE('',*,*,#5945,.F.);
#7458=ORIENTED_EDGE('',*,*,#5946,.F.);
#7459=ORIENTED_EDGE('',*,*,#5947,.F.);
#7460=ORIENTED_EDGE('',*,*,#5942,.F.);
#7461=ORIENTED_EDGE('',*,*,#5937,.T.);
#7462=ORIENTED_EDGE('',*,*,#5948,.F.);
#7463=ORIENTED_EDGE('',*,*,#5946,.T.);
#7464=ORIENTED_EDGE('',*,*,#5944,.F.);
#7465=ORIENTED_EDGE('',*,*,#5940,.T.);
#7466=ORIENTED_EDGE('',*,*,#5943,.F.);
#7467=ORIENTED_EDGE('',*,*,#5947,.T.);
#7468=ORIENTED_EDGE('',*,*,#5948,.T.);
#7469=ORIENTED_EDGE('',*,*,#5949,.T.);
#7470=ORIENTED_EDGE('',*,*,#5950,.T.);
#7471=ORIENTED_EDGE('',*,*,#5951,.F.);
#7472=ORIENTED_EDGE('',*,*,#5952,.F.);
#7473=ORIENTED_EDGE('',*,*,#5953,.T.);
#7474=ORIENTED_EDGE('',*,*,#5954,.T.);
#7475=ORIENTED_EDGE('',*,*,#5952,.T.);
#7476=ORIENTED_EDGE('',*,*,#5955,.F.);
#7477=ORIENTED_EDGE('',*,*,#5956,.T.);
#7478=ORIENTED_EDGE('',*,*,#5955,.T.);
#7479=ORIENTED_EDGE('',*,*,#5951,.T.);
#7480=ORIENTED_EDGE('',*,*,#5957,.T.);
#7481=ORIENTED_EDGE('',*,*,#5958,.T.);
#7482=ORIENTED_EDGE('',*,*,#5957,.F.);
#7483=ORIENTED_EDGE('',*,*,#5950,.F.);
#7484=ORIENTED_EDGE('',*,*,#5959,.T.);
#7485=ORIENTED_EDGE('',*,*,#5960,.T.);
#7486=ORIENTED_EDGE('',*,*,#5959,.F.);
#7487=ORIENTED_EDGE('',*,*,#5949,.F.);
#7488=ORIENTED_EDGE('',*,*,#5954,.F.);
#7489=ORIENTED_EDGE('',*,*,#5953,.F.);
#7490=ORIENTED_EDGE('',*,*,#5956,.F.);
#7491=ORIENTED_EDGE('',*,*,#5958,.F.);
#7492=ORIENTED_EDGE('',*,*,#5960,.F.);
#7493=ORIENTED_EDGE('',*,*,#5961,.F.);
#7494=ORIENTED_EDGE('',*,*,#5962,.T.);
#7495=ORIENTED_EDGE('',*,*,#5963,.F.);
#7496=ORIENTED_EDGE('',*,*,#5962,.F.);
#7497=ORIENTED_EDGE('',*,*,#5964,.F.);
#7498=ORIENTED_EDGE('',*,*,#5965,.T.);
#7499=ORIENTED_EDGE('',*,*,#5966,.F.);
#7500=ORIENTED_EDGE('',*,*,#5965,.F.);
#7501=ORIENTED_EDGE('',*,*,#5967,.F.);
#7502=ORIENTED_EDGE('',*,*,#5968,.T.);
#7503=ORIENTED_EDGE('',*,*,#5969,.F.);
#7504=ORIENTED_EDGE('',*,*,#5968,.F.);
#7505=ORIENTED_EDGE('',*,*,#5970,.F.);
#7506=ORIENTED_EDGE('',*,*,#5971,.T.);
#7507=ORIENTED_EDGE('',*,*,#5972,.F.);
#7508=ORIENTED_EDGE('',*,*,#5971,.F.);
#7509=ORIENTED_EDGE('',*,*,#5973,.F.);
#7510=ORIENTED_EDGE('',*,*,#5974,.T.);
#7511=ORIENTED_EDGE('',*,*,#5975,.F.);
#7512=ORIENTED_EDGE('',*,*,#5974,.F.);
#7513=ORIENTED_EDGE('',*,*,#5976,.F.);
#7514=ORIENTED_EDGE('',*,*,#5977,.T.);
#7515=ORIENTED_EDGE('',*,*,#5978,.F.);
#7516=ORIENTED_EDGE('',*,*,#5977,.F.);
#7517=ORIENTED_EDGE('',*,*,#5979,.F.);
#7518=ORIENTED_EDGE('',*,*,#5980,.T.);
#7519=ORIENTED_EDGE('',*,*,#5981,.F.);
#7520=ORIENTED_EDGE('',*,*,#5980,.F.);
#7521=ORIENTED_EDGE('',*,*,#5982,.F.);
#7522=ORIENTED_EDGE('',*,*,#5983,.T.);
#7523=ORIENTED_EDGE('',*,*,#5984,.F.);
#7524=ORIENTED_EDGE('',*,*,#5983,.F.);
#7525=ORIENTED_EDGE('',*,*,#5985,.F.);
#7526=ORIENTED_EDGE('',*,*,#5986,.T.);
#7527=ORIENTED_EDGE('',*,*,#5987,.F.);
#7528=ORIENTED_EDGE('',*,*,#5986,.F.);
#7529=ORIENTED_EDGE('',*,*,#5988,.F.);
#7530=ORIENTED_EDGE('',*,*,#5989,.F.);
#7531=ORIENTED_EDGE('',*,*,#5990,.T.);
#7532=ORIENTED_EDGE('',*,*,#5991,.F.);
#7533=ORIENTED_EDGE('',*,*,#5978,.T.);
#7534=ORIENTED_EDGE('',*,*,#5987,.T.);
#7535=ORIENTED_EDGE('',*,*,#5992,.F.);
#7536=ORIENTED_EDGE('',*,*,#5993,.F.);
#7537=ORIENTED_EDGE('',*,*,#5994,.F.);
#7538=ORIENTED_EDGE('',*,*,#5995,.F.);
#7539=ORIENTED_EDGE('',*,*,#5981,.T.);
#7540=ORIENTED_EDGE('',*,*,#5984,.T.);
#7541=ORIENTED_EDGE('',*,*,#5996,.F.);
#7542=ORIENTED_EDGE('',*,*,#5994,.T.);
#7543=ORIENTED_EDGE('',*,*,#5997,.F.);
#7544=ORIENTED_EDGE('',*,*,#5998,.F.);
#7545=ORIENTED_EDGE('',*,*,#5999,.F.);
#7546=ORIENTED_EDGE('',*,*,#6000,.T.);
#7547=ORIENTED_EDGE('',*,*,#6001,.F.);
#7548=ORIENTED_EDGE('',*,*,#5990,.F.);
#7549=ORIENTED_EDGE('',*,*,#6002,.T.);
#7550=ORIENTED_EDGE('',*,*,#6003,.F.);
#7551=ORIENTED_EDGE('',*,*,#6004,.F.);
#7552=ORIENTED_EDGE('',*,*,#5995,.T.);
#7553=ORIENTED_EDGE('',*,*,#5996,.T.);
#7554=ORIENTED_EDGE('',*,*,#6005,.T.);
#7555=ORIENTED_EDGE('',*,*,#5999,.T.);
#7556=ORIENTED_EDGE('',*,*,#5989,.T.);
#7557=ORIENTED_EDGE('',*,*,#5973,.T.);
#7558=ORIENTED_EDGE('',*,*,#5970,.T.);
#7559=ORIENTED_EDGE('',*,*,#5967,.T.);
#7560=ORIENTED_EDGE('',*,*,#5964,.T.);
#7561=ORIENTED_EDGE('',*,*,#5961,.T.);
#7562=ORIENTED_EDGE('',*,*,#5988,.T.);
#7563=ORIENTED_EDGE('',*,*,#6006,.T.);
#7564=ORIENTED_EDGE('',*,*,#6007,.F.);
#7565=ORIENTED_EDGE('',*,*,#6002,.F.);
#7566=ORIENTED_EDGE('',*,*,#6008,.T.);
#7567=ORIENTED_EDGE('',*,*,#6009,.F.);
#7568=ORIENTED_EDGE('',*,*,#6006,.F.);
#7569=ORIENTED_EDGE('',*,*,#5991,.T.);
#7570=ORIENTED_EDGE('',*,*,#6001,.T.);
#7571=ORIENTED_EDGE('',*,*,#6010,.T.);
#7572=ORIENTED_EDGE('',*,*,#5997,.T.);
#7573=ORIENTED_EDGE('',*,*,#5993,.T.);
#7574=ORIENTED_EDGE('',*,*,#5975,.T.);
#7575=ORIENTED_EDGE('',*,*,#5972,.T.);
#7576=ORIENTED_EDGE('',*,*,#5969,.T.);
#7577=ORIENTED_EDGE('',*,*,#5966,.T.);
#7578=ORIENTED_EDGE('',*,*,#5963,.T.);
#7579=ORIENTED_EDGE('',*,*,#5992,.T.);
#7580=ORIENTED_EDGE('',*,*,#6004,.T.);
#7581=ORIENTED_EDGE('',*,*,#6011,.F.);
#7582=ORIENTED_EDGE('',*,*,#6008,.F.);
#7583=ORIENTED_EDGE('',*,*,#6011,.T.);
#7584=ORIENTED_EDGE('',*,*,#6003,.T.);
#7585=ORIENTED_EDGE('',*,*,#6007,.T.);
#7586=ORIENTED_EDGE('',*,*,#6009,.T.);
#7587=ORIENTED_EDGE('',*,*,#6010,.F.);
#7588=ORIENTED_EDGE('',*,*,#6000,.F.);
#7589=ORIENTED_EDGE('',*,*,#6005,.F.);
#7590=ORIENTED_EDGE('',*,*,#5998,.T.);
#7591=ORIENTED_EDGE('',*,*,#5976,.T.);
#7592=ORIENTED_EDGE('',*,*,#5979,.T.);
#7593=ORIENTED_EDGE('',*,*,#5982,.T.);
#7594=ORIENTED_EDGE('',*,*,#5985,.T.);
#7595=ORIENTED_EDGE('',*,*,#6012,.F.);
#7596=ORIENTED_EDGE('',*,*,#6013,.T.);
#7597=ORIENTED_EDGE('',*,*,#6014,.T.);
#7598=ORIENTED_EDGE('',*,*,#6013,.F.);
#7599=ORIENTED_EDGE('',*,*,#6015,.F.);
#7600=ORIENTED_EDGE('',*,*,#6016,.T.);
#7601=ORIENTED_EDGE('',*,*,#6017,.T.);
#7602=ORIENTED_EDGE('',*,*,#6016,.F.);
#7603=ORIENTED_EDGE('',*,*,#6015,.T.);
#7604=ORIENTED_EDGE('',*,*,#6012,.T.);
#7605=ORIENTED_EDGE('',*,*,#6017,.F.);
#7606=ORIENTED_EDGE('',*,*,#6014,.F.);
#7607=ORIENTED_EDGE('',*,*,#6018,.F.);
#7608=ORIENTED_EDGE('',*,*,#6019,.F.);
#7609=ORIENTED_EDGE('',*,*,#6020,.F.);
#7610=ORIENTED_EDGE('',*,*,#6021,.F.);
#7611=ORIENTED_EDGE('',*,*,#6022,.F.);
#7612=ORIENTED_EDGE('',*,*,#6023,.F.);
#7613=ORIENTED_EDGE('',*,*,#6024,.F.);
#7614=ORIENTED_EDGE('',*,*,#6025,.F.);
#7615=ORIENTED_EDGE('',*,*,#6026,.F.);
#7616=ORIENTED_EDGE('',*,*,#6027,.F.);
#7617=ORIENTED_EDGE('',*,*,#6028,.F.);
#7618=ORIENTED_EDGE('',*,*,#6029,.F.);
#7619=ORIENTED_EDGE('',*,*,#6030,.F.);
#7620=ORIENTED_EDGE('',*,*,#6031,.F.);
#7621=ORIENTED_EDGE('',*,*,#6032,.F.);
#7622=ORIENTED_EDGE('',*,*,#6033,.F.);
#7623=ORIENTED_EDGE('',*,*,#6019,.T.);
#7624=ORIENTED_EDGE('',*,*,#6034,.F.);
#7625=ORIENTED_EDGE('',*,*,#6031,.T.);
#7626=ORIENTED_EDGE('',*,*,#6035,.F.);
#7627=ORIENTED_EDGE('',*,*,#6027,.T.);
#7628=ORIENTED_EDGE('',*,*,#6036,.F.);
#7629=ORIENTED_EDGE('',*,*,#6023,.T.);
#7630=ORIENTED_EDGE('',*,*,#6037,.F.);
#7631=ORIENTED_EDGE('',*,*,#6038,.F.);
#7632=ORIENTED_EDGE('',*,*,#6028,.T.);
#7633=ORIENTED_EDGE('',*,*,#6035,.T.);
#7634=ORIENTED_EDGE('',*,*,#6030,.T.);
#7635=ORIENTED_EDGE('',*,*,#6039,.F.);
#7636=ORIENTED_EDGE('',*,*,#6024,.T.);
#7637=ORIENTED_EDGE('',*,*,#6036,.T.);
#7638=ORIENTED_EDGE('',*,*,#6026,.T.);
#7639=ORIENTED_EDGE('',*,*,#6040,.F.);
#7640=ORIENTED_EDGE('',*,*,#6018,.T.);
#7641=ORIENTED_EDGE('',*,*,#6041,.F.);
#7642=ORIENTED_EDGE('',*,*,#6032,.T.);
#7643=ORIENTED_EDGE('',*,*,#6034,.T.);
#7644=ORIENTED_EDGE('',*,*,#6020,.T.);
#7645=ORIENTED_EDGE('',*,*,#6037,.T.);
#7646=ORIENTED_EDGE('',*,*,#6022,.T.);
#7647=ORIENTED_EDGE('',*,*,#6042,.F.);
#7648=ORIENTED_EDGE('',*,*,#6043,.F.);
#7649=ORIENTED_EDGE('',*,*,#6044,.T.);
#7650=ORIENTED_EDGE('',*,*,#6045,.F.);
#7651=ORIENTED_EDGE('',*,*,#6044,.F.);
#7652=ORIENTED_EDGE('',*,*,#6043,.T.);
#7653=ORIENTED_EDGE('',*,*,#6046,.T.);
#7654=ORIENTED_EDGE('',*,*,#6046,.F.);
#7655=ORIENTED_EDGE('',*,*,#6047,.T.);
#7656=ORIENTED_EDGE('',*,*,#6038,.T.);
#7657=ORIENTED_EDGE('',*,*,#6047,.F.);
#7658=ORIENTED_EDGE('',*,*,#6021,.T.);
#7659=ORIENTED_EDGE('',*,*,#6042,.T.);
#7660=ORIENTED_EDGE('',*,*,#6025,.T.);
#7661=ORIENTED_EDGE('',*,*,#6040,.T.);
#7662=ORIENTED_EDGE('',*,*,#6029,.T.);
#7663=ORIENTED_EDGE('',*,*,#6039,.T.);
#7664=ORIENTED_EDGE('',*,*,#6033,.T.);
#7665=ORIENTED_EDGE('',*,*,#6041,.T.);
#7666=ORIENTED_EDGE('',*,*,#6045,.T.);
#7667=ORIENTED_EDGE('',*,*,#6048,.F.);
#7668=ORIENTED_EDGE('',*,*,#6049,.F.);
#7669=ORIENTED_EDGE('',*,*,#6050,.F.);
#7670=ORIENTED_EDGE('',*,*,#6051,.F.);
#7671=ORIENTED_EDGE('',*,*,#6052,.F.);
#7672=ORIENTED_EDGE('',*,*,#6053,.F.);
#7673=ORIENTED_EDGE('',*,*,#6054,.F.);
#7674=ORIENTED_EDGE('',*,*,#6055,.F.);
#7675=ORIENTED_EDGE('',*,*,#6056,.F.);
#7676=ORIENTED_EDGE('',*,*,#6057,.F.);
#7677=ORIENTED_EDGE('',*,*,#6058,.F.);
#7678=ORIENTED_EDGE('',*,*,#6059,.F.);
#7679=ORIENTED_EDGE('',*,*,#6060,.F.);
#7680=ORIENTED_EDGE('',*,*,#6061,.F.);
#7681=ORIENTED_EDGE('',*,*,#6062,.F.);
#7682=ORIENTED_EDGE('',*,*,#6063,.F.);
#7683=ORIENTED_EDGE('',*,*,#6049,.T.);
#7684=ORIENTED_EDGE('',*,*,#6064,.F.);
#7685=ORIENTED_EDGE('',*,*,#6061,.T.);
#7686=ORIENTED_EDGE('',*,*,#6065,.F.);
#7687=ORIENTED_EDGE('',*,*,#6057,.T.);
#7688=ORIENTED_EDGE('',*,*,#6066,.F.);
#7689=ORIENTED_EDGE('',*,*,#6053,.T.);
#7690=ORIENTED_EDGE('',*,*,#6067,.F.);
#7691=ORIENTED_EDGE('',*,*,#6068,.T.);
#7692=ORIENTED_EDGE('',*,*,#6058,.T.);
#7693=ORIENTED_EDGE('',*,*,#6065,.T.);
#7694=ORIENTED_EDGE('',*,*,#6060,.T.);
#7695=ORIENTED_EDGE('',*,*,#6069,.F.);
#7696=ORIENTED_EDGE('',*,*,#6054,.T.);
#7697=ORIENTED_EDGE('',*,*,#6066,.T.);
#7698=ORIENTED_EDGE('',*,*,#6056,.T.);
#7699=ORIENTED_EDGE('',*,*,#6070,.F.);
#7700=ORIENTED_EDGE('',*,*,#6048,.T.);
#7701=ORIENTED_EDGE('',*,*,#6071,.F.);
#7702=ORIENTED_EDGE('',*,*,#6062,.T.);
#7703=ORIENTED_EDGE('',*,*,#6064,.T.);
#7704=ORIENTED_EDGE('',*,*,#6050,.T.);
#7705=ORIENTED_EDGE('',*,*,#6067,.T.);
#7706=ORIENTED_EDGE('',*,*,#6052,.T.);
#7707=ORIENTED_EDGE('',*,*,#6072,.F.);
#7708=ORIENTED_EDGE('',*,*,#6068,.F.);
#7709=ORIENTED_EDGE('',*,*,#6073,.T.);
#7710=ORIENTED_EDGE('',*,*,#6074,.T.);
#7711=ORIENTED_EDGE('',*,*,#6073,.F.);
#7712=ORIENTED_EDGE('',*,*,#6074,.F.);
#7713=ORIENTED_EDGE('',*,*,#6075,.F.);
#7714=ORIENTED_EDGE('',*,*,#6076,.F.);
#7715=ORIENTED_EDGE('',*,*,#6077,.T.);
#7716=ORIENTED_EDGE('',*,*,#6075,.T.);
#7717=ORIENTED_EDGE('',*,*,#6077,.F.);
#7718=ORIENTED_EDGE('',*,*,#6051,.T.);
#7719=ORIENTED_EDGE('',*,*,#6072,.T.);
#7720=ORIENTED_EDGE('',*,*,#6055,.T.);
#7721=ORIENTED_EDGE('',*,*,#6070,.T.);
#7722=ORIENTED_EDGE('',*,*,#6059,.T.);
#7723=ORIENTED_EDGE('',*,*,#6069,.T.);
#7724=ORIENTED_EDGE('',*,*,#6063,.T.);
#7725=ORIENTED_EDGE('',*,*,#6071,.T.);
#7726=ORIENTED_EDGE('',*,*,#6076,.T.);
#7727=ORIENTED_EDGE('',*,*,#6078,.F.);
#7728=ORIENTED_EDGE('',*,*,#6079,.T.);
#7729=ORIENTED_EDGE('',*,*,#6080,.F.);
#7730=ORIENTED_EDGE('',*,*,#6079,.F.);
#7731=ORIENTED_EDGE('',*,*,#6081,.F.);
#7732=ORIENTED_EDGE('',*,*,#6082,.T.);
#7733=ORIENTED_EDGE('',*,*,#6083,.F.);
#7734=ORIENTED_EDGE('',*,*,#6082,.F.);
#7735=ORIENTED_EDGE('',*,*,#6084,.F.);
#7736=ORIENTED_EDGE('',*,*,#6085,.T.);
#7737=ORIENTED_EDGE('',*,*,#6086,.F.);
#7738=ORIENTED_EDGE('',*,*,#6085,.F.);
#7739=ORIENTED_EDGE('',*,*,#6087,.F.);
#7740=ORIENTED_EDGE('',*,*,#6088,.T.);
#7741=ORIENTED_EDGE('',*,*,#6089,.F.);
#7742=ORIENTED_EDGE('',*,*,#6088,.F.);
#7743=ORIENTED_EDGE('',*,*,#6090,.F.);
#7744=ORIENTED_EDGE('',*,*,#6091,.T.);
#7745=ORIENTED_EDGE('',*,*,#6092,.F.);
#7746=ORIENTED_EDGE('',*,*,#6091,.F.);
#7747=ORIENTED_EDGE('',*,*,#6093,.F.);
#7748=ORIENTED_EDGE('',*,*,#6094,.T.);
#7749=ORIENTED_EDGE('',*,*,#6095,.F.);
#7750=ORIENTED_EDGE('',*,*,#6094,.F.);
#7751=ORIENTED_EDGE('',*,*,#6096,.F.);
#7752=ORIENTED_EDGE('',*,*,#6097,.T.);
#7753=ORIENTED_EDGE('',*,*,#6098,.F.);
#7754=ORIENTED_EDGE('',*,*,#6097,.F.);
#7755=ORIENTED_EDGE('',*,*,#6099,.F.);
#7756=ORIENTED_EDGE('',*,*,#6100,.T.);
#7757=ORIENTED_EDGE('',*,*,#6101,.F.);
#7758=ORIENTED_EDGE('',*,*,#6100,.F.);
#7759=ORIENTED_EDGE('',*,*,#6102,.F.);
#7760=ORIENTED_EDGE('',*,*,#6103,.T.);
#7761=ORIENTED_EDGE('',*,*,#6104,.F.);
#7762=ORIENTED_EDGE('',*,*,#6103,.F.);
#7763=ORIENTED_EDGE('',*,*,#6105,.F.);
#7764=ORIENTED_EDGE('',*,*,#6106,.F.);
#7765=ORIENTED_EDGE('',*,*,#6107,.T.);
#7766=ORIENTED_EDGE('',*,*,#6108,.F.);
#7767=ORIENTED_EDGE('',*,*,#6095,.T.);
#7768=ORIENTED_EDGE('',*,*,#6104,.T.);
#7769=ORIENTED_EDGE('',*,*,#6109,.F.);
#7770=ORIENTED_EDGE('',*,*,#6110,.F.);
#7771=ORIENTED_EDGE('',*,*,#6111,.F.);
#7772=ORIENTED_EDGE('',*,*,#6112,.F.);
#7773=ORIENTED_EDGE('',*,*,#6098,.T.);
#7774=ORIENTED_EDGE('',*,*,#6101,.T.);
#7775=ORIENTED_EDGE('',*,*,#6113,.F.);
#7776=ORIENTED_EDGE('',*,*,#6111,.T.);
#7777=ORIENTED_EDGE('',*,*,#6114,.F.);
#7778=ORIENTED_EDGE('',*,*,#6115,.F.);
#7779=ORIENTED_EDGE('',*,*,#6116,.F.);
#7780=ORIENTED_EDGE('',*,*,#6117,.T.);
#7781=ORIENTED_EDGE('',*,*,#6118,.F.);
#7782=ORIENTED_EDGE('',*,*,#6107,.F.);
#7783=ORIENTED_EDGE('',*,*,#6119,.T.);
#7784=ORIENTED_EDGE('',*,*,#6120,.F.);
#7785=ORIENTED_EDGE('',*,*,#6121,.F.);
#7786=ORIENTED_EDGE('',*,*,#6112,.T.);
#7787=ORIENTED_EDGE('',*,*,#6113,.T.);
#7788=ORIENTED_EDGE('',*,*,#6122,.T.);
#7789=ORIENTED_EDGE('',*,*,#6116,.T.);
#7790=ORIENTED_EDGE('',*,*,#6106,.T.);
#7791=ORIENTED_EDGE('',*,*,#6090,.T.);
#7792=ORIENTED_EDGE('',*,*,#6087,.T.);
#7793=ORIENTED_EDGE('',*,*,#6084,.T.);
#7794=ORIENTED_EDGE('',*,*,#6081,.T.);
#7795=ORIENTED_EDGE('',*,*,#6078,.T.);
#7796=ORIENTED_EDGE('',*,*,#6105,.T.);
#7797=ORIENTED_EDGE('',*,*,#6123,.T.);
#7798=ORIENTED_EDGE('',*,*,#6124,.F.);
#7799=ORIENTED_EDGE('',*,*,#6119,.F.);
#7800=ORIENTED_EDGE('',*,*,#6125,.T.);
#7801=ORIENTED_EDGE('',*,*,#6126,.F.);
#7802=ORIENTED_EDGE('',*,*,#6123,.F.);
#7803=ORIENTED_EDGE('',*,*,#6108,.T.);
#7804=ORIENTED_EDGE('',*,*,#6118,.T.);
#7805=ORIENTED_EDGE('',*,*,#6127,.T.);
#7806=ORIENTED_EDGE('',*,*,#6114,.T.);
#7807=ORIENTED_EDGE('',*,*,#6110,.T.);
#7808=ORIENTED_EDGE('',*,*,#6092,.T.);
#7809=ORIENTED_EDGE('',*,*,#6089,.T.);
#7810=ORIENTED_EDGE('',*,*,#6086,.T.);
#7811=ORIENTED_EDGE('',*,*,#6083,.T.);
#7812=ORIENTED_EDGE('',*,*,#6080,.T.);
#7813=ORIENTED_EDGE('',*,*,#6109,.T.);
#7814=ORIENTED_EDGE('',*,*,#6121,.T.);
#7815=ORIENTED_EDGE('',*,*,#6128,.F.);
#7816=ORIENTED_EDGE('',*,*,#6125,.F.);
#7817=ORIENTED_EDGE('',*,*,#6128,.T.);
#7818=ORIENTED_EDGE('',*,*,#6120,.T.);
#7819=ORIENTED_EDGE('',*,*,#6124,.T.);
#7820=ORIENTED_EDGE('',*,*,#6126,.T.);
#7821=ORIENTED_EDGE('',*,*,#6127,.F.);
#7822=ORIENTED_EDGE('',*,*,#6117,.F.);
#7823=ORIENTED_EDGE('',*,*,#6122,.F.);
#7824=ORIENTED_EDGE('',*,*,#6115,.T.);
#7825=ORIENTED_EDGE('',*,*,#6093,.T.);
#7826=ORIENTED_EDGE('',*,*,#6096,.T.);
#7827=ORIENTED_EDGE('',*,*,#6099,.T.);
#7828=ORIENTED_EDGE('',*,*,#6102,.T.);
#7829=ORIENTED_EDGE('',*,*,#6129,.F.);
#7830=ORIENTED_EDGE('',*,*,#6130,.T.);
#7831=ORIENTED_EDGE('',*,*,#6131,.T.);
#7832=ORIENTED_EDGE('',*,*,#6130,.F.);
#7833=ORIENTED_EDGE('',*,*,#6132,.F.);
#7834=ORIENTED_EDGE('',*,*,#6133,.T.);
#7835=ORIENTED_EDGE('',*,*,#6134,.T.);
#7836=ORIENTED_EDGE('',*,*,#6133,.F.);
#7837=ORIENTED_EDGE('',*,*,#6132,.T.);
#7838=ORIENTED_EDGE('',*,*,#6129,.T.);
#7839=ORIENTED_EDGE('',*,*,#6134,.F.);
#7840=ORIENTED_EDGE('',*,*,#6131,.F.);
#7841=ORIENTED_EDGE('',*,*,#6135,.F.);
#7842=ORIENTED_EDGE('',*,*,#6136,.F.);
#7843=ORIENTED_EDGE('',*,*,#6137,.F.);
#7844=ORIENTED_EDGE('',*,*,#6138,.F.);
#7845=ORIENTED_EDGE('',*,*,#6139,.F.);
#7846=ORIENTED_EDGE('',*,*,#6140,.F.);
#7847=ORIENTED_EDGE('',*,*,#6141,.F.);
#7848=ORIENTED_EDGE('',*,*,#6142,.F.);
#7849=ORIENTED_EDGE('',*,*,#6143,.F.);
#7850=ORIENTED_EDGE('',*,*,#6144,.F.);
#7851=ORIENTED_EDGE('',*,*,#6145,.F.);
#7852=ORIENTED_EDGE('',*,*,#6146,.F.);
#7853=ORIENTED_EDGE('',*,*,#6147,.F.);
#7854=ORIENTED_EDGE('',*,*,#6148,.F.);
#7855=ORIENTED_EDGE('',*,*,#6149,.F.);
#7856=ORIENTED_EDGE('',*,*,#6150,.F.);
#7857=ORIENTED_EDGE('',*,*,#6136,.T.);
#7858=ORIENTED_EDGE('',*,*,#6151,.F.);
#7859=ORIENTED_EDGE('',*,*,#6148,.T.);
#7860=ORIENTED_EDGE('',*,*,#6152,.F.);
#7861=ORIENTED_EDGE('',*,*,#6144,.T.);
#7862=ORIENTED_EDGE('',*,*,#6153,.F.);
#7863=ORIENTED_EDGE('',*,*,#6140,.T.);
#7864=ORIENTED_EDGE('',*,*,#6154,.F.);
#7865=ORIENTED_EDGE('',*,*,#6155,.F.);
#7866=ORIENTED_EDGE('',*,*,#6145,.T.);
#7867=ORIENTED_EDGE('',*,*,#6152,.T.);
#7868=ORIENTED_EDGE('',*,*,#6147,.T.);
#7869=ORIENTED_EDGE('',*,*,#6156,.F.);
#7870=ORIENTED_EDGE('',*,*,#6141,.T.);
#7871=ORIENTED_EDGE('',*,*,#6153,.T.);
#7872=ORIENTED_EDGE('',*,*,#6143,.T.);
#7873=ORIENTED_EDGE('',*,*,#6157,.F.);
#7874=ORIENTED_EDGE('',*,*,#6135,.T.);
#7875=ORIENTED_EDGE('',*,*,#6158,.F.);
#7876=ORIENTED_EDGE('',*,*,#6149,.T.);
#7877=ORIENTED_EDGE('',*,*,#6151,.T.);
#7878=ORIENTED_EDGE('',*,*,#6137,.T.);
#7879=ORIENTED_EDGE('',*,*,#6154,.T.);
#7880=ORIENTED_EDGE('',*,*,#6139,.T.);
#7881=ORIENTED_EDGE('',*,*,#6159,.F.);
#7882=ORIENTED_EDGE('',*,*,#6160,.F.);
#7883=ORIENTED_EDGE('',*,*,#6161,.T.);
#7884=ORIENTED_EDGE('',*,*,#6162,.F.);
#7885=ORIENTED_EDGE('',*,*,#6161,.F.);
#7886=ORIENTED_EDGE('',*,*,#6160,.T.);
#7887=ORIENTED_EDGE('',*,*,#6163,.T.);
#7888=ORIENTED_EDGE('',*,*,#6163,.F.);
#7889=ORIENTED_EDGE('',*,*,#6164,.T.);
#7890=ORIENTED_EDGE('',*,*,#6155,.T.);
#7891=ORIENTED_EDGE('',*,*,#6164,.F.);
#7892=ORIENTED_EDGE('',*,*,#6138,.T.);
#7893=ORIENTED_EDGE('',*,*,#6159,.T.);
#7894=ORIENTED_EDGE('',*,*,#6142,.T.);
#7895=ORIENTED_EDGE('',*,*,#6157,.T.);
#7896=ORIENTED_EDGE('',*,*,#6146,.T.);
#7897=ORIENTED_EDGE('',*,*,#6156,.T.);
#7898=ORIENTED_EDGE('',*,*,#6150,.T.);
#7899=ORIENTED_EDGE('',*,*,#6158,.T.);
#7900=ORIENTED_EDGE('',*,*,#6162,.T.);
#7901=ORIENTED_EDGE('',*,*,#6165,.F.);
#7902=ORIENTED_EDGE('',*,*,#6166,.F.);
#7903=ORIENTED_EDGE('',*,*,#6167,.F.);
#7904=ORIENTED_EDGE('',*,*,#6168,.F.);
#7905=ORIENTED_EDGE('',*,*,#6169,.F.);
#7906=ORIENTED_EDGE('',*,*,#6170,.F.);
#7907=ORIENTED_EDGE('',*,*,#6171,.F.);
#7908=ORIENTED_EDGE('',*,*,#6172,.F.);
#7909=ORIENTED_EDGE('',*,*,#6173,.F.);
#7910=ORIENTED_EDGE('',*,*,#6174,.F.);
#7911=ORIENTED_EDGE('',*,*,#6175,.F.);
#7912=ORIENTED_EDGE('',*,*,#6176,.F.);
#7913=ORIENTED_EDGE('',*,*,#6177,.F.);
#7914=ORIENTED_EDGE('',*,*,#6178,.F.);
#7915=ORIENTED_EDGE('',*,*,#6179,.F.);
#7916=ORIENTED_EDGE('',*,*,#6180,.F.);
#7917=ORIENTED_EDGE('',*,*,#6166,.T.);
#7918=ORIENTED_EDGE('',*,*,#6181,.F.);
#7919=ORIENTED_EDGE('',*,*,#6178,.T.);
#7920=ORIENTED_EDGE('',*,*,#6182,.F.);
#7921=ORIENTED_EDGE('',*,*,#6174,.T.);
#7922=ORIENTED_EDGE('',*,*,#6183,.F.);
#7923=ORIENTED_EDGE('',*,*,#6170,.T.);
#7924=ORIENTED_EDGE('',*,*,#6184,.F.);
#7925=ORIENTED_EDGE('',*,*,#6185,.T.);
#7926=ORIENTED_EDGE('',*,*,#6175,.T.);
#7927=ORIENTED_EDGE('',*,*,#6182,.T.);
#7928=ORIENTED_EDGE('',*,*,#6177,.T.);
#7929=ORIENTED_EDGE('',*,*,#6186,.F.);
#7930=ORIENTED_EDGE('',*,*,#6171,.T.);
#7931=ORIENTED_EDGE('',*,*,#6183,.T.);
#7932=ORIENTED_EDGE('',*,*,#6173,.T.);
#7933=ORIENTED_EDGE('',*,*,#6187,.F.);
#7934=ORIENTED_EDGE('',*,*,#6165,.T.);
#7935=ORIENTED_EDGE('',*,*,#6188,.F.);
#7936=ORIENTED_EDGE('',*,*,#6179,.T.);
#7937=ORIENTED_EDGE('',*,*,#6181,.T.);
#7938=ORIENTED_EDGE('',*,*,#6167,.T.);
#7939=ORIENTED_EDGE('',*,*,#6184,.T.);
#7940=ORIENTED_EDGE('',*,*,#6169,.T.);
#7941=ORIENTED_EDGE('',*,*,#6189,.F.);
#7942=ORIENTED_EDGE('',*,*,#6185,.F.);
#7943=ORIENTED_EDGE('',*,*,#6190,.T.);
#7944=ORIENTED_EDGE('',*,*,#6191,.T.);
#7945=ORIENTED_EDGE('',*,*,#6190,.F.);
#7946=ORIENTED_EDGE('',*,*,#6191,.F.);
#7947=ORIENTED_EDGE('',*,*,#6192,.F.);
#7948=ORIENTED_EDGE('',*,*,#6193,.F.);
#7949=ORIENTED_EDGE('',*,*,#6194,.T.);
#7950=ORIENTED_EDGE('',*,*,#6192,.T.);
#7951=ORIENTED_EDGE('',*,*,#6194,.F.);
#7952=ORIENTED_EDGE('',*,*,#6168,.T.);
#7953=ORIENTED_EDGE('',*,*,#6189,.T.);
#7954=ORIENTED_EDGE('',*,*,#6172,.T.);
#7955=ORIENTED_EDGE('',*,*,#6187,.T.);
#7956=ORIENTED_EDGE('',*,*,#6176,.T.);
#7957=ORIENTED_EDGE('',*,*,#6186,.T.);
#7958=ORIENTED_EDGE('',*,*,#6180,.T.);
#7959=ORIENTED_EDGE('',*,*,#6188,.T.);
#7960=ORIENTED_EDGE('',*,*,#6193,.T.);
#7961=ORIENTED_EDGE('',*,*,#6195,.F.);
#7962=ORIENTED_EDGE('',*,*,#6196,.F.);
#7963=ORIENTED_EDGE('',*,*,#6197,.F.);
#7964=ORIENTED_EDGE('',*,*,#6198,.T.);
#7965=ORIENTED_EDGE('',*,*,#6199,.F.);
#7966=ORIENTED_EDGE('',*,*,#6200,.F.);
#7967=ORIENTED_EDGE('',*,*,#6201,.F.);
#7968=ORIENTED_EDGE('',*,*,#6202,.F.);
#7969=ORIENTED_EDGE('',*,*,#6203,.F.);
#7970=ORIENTED_EDGE('',*,*,#6204,.F.);
#7971=ORIENTED_EDGE('',*,*,#6205,.F.);
#7972=ORIENTED_EDGE('',*,*,#6206,.F.);
#7973=ORIENTED_EDGE('',*,*,#6195,.T.);
#7974=ORIENTED_EDGE('',*,*,#6207,.T.);
#7975=ORIENTED_EDGE('',*,*,#6199,.T.);
#7976=ORIENTED_EDGE('',*,*,#6208,.T.);
#7977=ORIENTED_EDGE('',*,*,#6198,.F.);
#7978=ORIENTED_EDGE('',*,*,#6209,.F.);
#7979=ORIENTED_EDGE('',*,*,#6200,.T.);
#7980=ORIENTED_EDGE('',*,*,#6207,.F.);
#7981=ORIENTED_EDGE('',*,*,#6196,.T.);
#7982=ORIENTED_EDGE('',*,*,#6208,.F.);
#7983=ORIENTED_EDGE('',*,*,#6202,.T.);
#7984=ORIENTED_EDGE('',*,*,#6210,.F.);
#7985=ORIENTED_EDGE('',*,*,#6211,.T.);
#7986=ORIENTED_EDGE('',*,*,#6212,.F.);
#7987=ORIENTED_EDGE('',*,*,#6213,.F.);
#7988=ORIENTED_EDGE('',*,*,#6206,.T.);
#7989=ORIENTED_EDGE('',*,*,#6205,.T.);
#7990=ORIENTED_EDGE('',*,*,#6214,.T.);
#7991=ORIENTED_EDGE('',*,*,#6215,.F.);
#7992=ORIENTED_EDGE('',*,*,#6211,.F.);
#7993=ORIENTED_EDGE('',*,*,#6203,.T.);
#7994=ORIENTED_EDGE('',*,*,#6213,.T.);
#7995=ORIENTED_EDGE('',*,*,#6216,.F.);
#7996=ORIENTED_EDGE('',*,*,#6217,.F.);
#7997=ORIENTED_EDGE('',*,*,#6214,.F.);
#7998=ORIENTED_EDGE('',*,*,#6204,.T.);
#7999=ORIENTED_EDGE('',*,*,#6217,.T.);
#8000=ORIENTED_EDGE('',*,*,#6218,.F.);
#8001=ORIENTED_EDGE('',*,*,#6215,.T.);
#8002=ORIENTED_EDGE('',*,*,#6218,.T.);
#8003=ORIENTED_EDGE('',*,*,#6216,.T.);
#8004=ORIENTED_EDGE('',*,*,#6212,.T.);
#8005=ORIENTED_EDGE('',*,*,#6197,.T.);
#8006=ORIENTED_EDGE('',*,*,#6210,.T.);
#8007=ORIENTED_EDGE('',*,*,#6201,.T.);
#8008=ORIENTED_EDGE('',*,*,#6209,.T.);
#8009=ORIENTED_EDGE('',*,*,#6219,.F.);
#8010=ORIENTED_EDGE('',*,*,#6220,.F.);
#8011=ORIENTED_EDGE('',*,*,#6221,.F.);
#8012=ORIENTED_EDGE('',*,*,#6222,.F.);
#8013=ORIENTED_EDGE('',*,*,#6223,.F.);
#8014=ORIENTED_EDGE('',*,*,#6224,.F.);
#8015=ORIENTED_EDGE('',*,*,#6225,.F.);
#8016=ORIENTED_EDGE('',*,*,#6226,.F.);
#8017=ORIENTED_EDGE('',*,*,#6227,.F.);
#8018=ORIENTED_EDGE('',*,*,#6222,.T.);
#8019=ORIENTED_EDGE('',*,*,#6228,.F.);
#8020=ORIENTED_EDGE('',*,*,#6224,.T.);
#8021=ORIENTED_EDGE('',*,*,#6229,.F.);
#8022=ORIENTED_EDGE('',*,*,#6230,.F.);
#8023=ORIENTED_EDGE('',*,*,#6231,.F.);
#8024=ORIENTED_EDGE('',*,*,#6232,.F.);
#8025=ORIENTED_EDGE('',*,*,#6233,.F.);
#8026=ORIENTED_EDGE('',*,*,#6234,.F.);
#8027=ORIENTED_EDGE('',*,*,#6235,.F.);
#8028=ORIENTED_EDGE('',*,*,#6236,.F.);
#8029=ORIENTED_EDGE('',*,*,#6237,.F.);
#8030=ORIENTED_EDGE('',*,*,#6238,.F.);
#8031=ORIENTED_EDGE('',*,*,#6233,.T.);
#8032=ORIENTED_EDGE('',*,*,#6239,.F.);
#8033=ORIENTED_EDGE('',*,*,#6235,.T.);
#8034=ORIENTED_EDGE('',*,*,#6240,.F.);
#8035=ORIENTED_EDGE('',*,*,#6225,.T.);
#8036=ORIENTED_EDGE('',*,*,#6228,.T.);
#8037=ORIENTED_EDGE('',*,*,#6221,.T.);
#8038=ORIENTED_EDGE('',*,*,#6241,.F.);
#8039=ORIENTED_EDGE('',*,*,#6242,.F.);
#8040=ORIENTED_EDGE('',*,*,#6243,.T.);
#8041=ORIENTED_EDGE('',*,*,#6244,.T.);
#8042=ORIENTED_EDGE('',*,*,#6245,.T.);
#8043=ORIENTED_EDGE('',*,*,#6246,.T.);
#8044=ORIENTED_EDGE('',*,*,#6247,.T.);
#8045=ORIENTED_EDGE('',*,*,#6248,.T.);
#8046=ORIENTED_EDGE('',*,*,#6249,.F.);
#8047=ORIENTED_EDGE('',*,*,#6236,.T.);
#8048=ORIENTED_EDGE('',*,*,#6239,.T.);
#8049=ORIENTED_EDGE('',*,*,#6232,.T.);
#8050=ORIENTED_EDGE('',*,*,#6250,.F.);
#8051=ORIENTED_EDGE('',*,*,#6237,.T.);
#8052=ORIENTED_EDGE('',*,*,#6249,.T.);
#8053=ORIENTED_EDGE('',*,*,#6251,.T.);
#8054=ORIENTED_EDGE('',*,*,#6252,.T.);
#8055=ORIENTED_EDGE('',*,*,#6220,.T.);
#8056=ORIENTED_EDGE('',*,*,#6253,.T.);
#8057=ORIENTED_EDGE('',*,*,#6254,.T.);
#8058=ORIENTED_EDGE('',*,*,#6241,.T.);
#8059=ORIENTED_EDGE('',*,*,#6226,.T.);
#8060=ORIENTED_EDGE('',*,*,#6250,.T.);
#8061=ORIENTED_EDGE('',*,*,#6231,.T.);
#8062=ORIENTED_EDGE('',*,*,#6255,.T.);
#8063=ORIENTED_EDGE('',*,*,#6256,.F.);
#8064=ORIENTED_EDGE('',*,*,#6257,.T.);
#8065=ORIENTED_EDGE('',*,*,#6229,.T.);
#8066=ORIENTED_EDGE('',*,*,#6257,.F.);
#8067=ORIENTED_EDGE('',*,*,#6258,.F.);
#8068=ORIENTED_EDGE('',*,*,#6259,.T.);
#8069=ORIENTED_EDGE('',*,*,#6240,.T.);
#8070=ORIENTED_EDGE('',*,*,#6259,.F.);
#8071=ORIENTED_EDGE('',*,*,#6246,.F.);
#8072=ORIENTED_EDGE('',*,*,#6260,.T.);
#8073=ORIENTED_EDGE('',*,*,#6261,.F.);
#8074=ORIENTED_EDGE('',*,*,#6262,.F.);
#8075=ORIENTED_EDGE('',*,*,#6244,.F.);
#8076=ORIENTED_EDGE('',*,*,#6263,.F.);
#8077=ORIENTED_EDGE('',*,*,#6264,.F.);
#8078=ORIENTED_EDGE('',*,*,#6265,.T.);
#8079=ORIENTED_EDGE('',*,*,#6245,.F.);
#8080=ORIENTED_EDGE('',*,*,#6265,.F.);
#8081=ORIENTED_EDGE('',*,*,#6266,.F.);
#8082=ORIENTED_EDGE('',*,*,#6260,.F.);
#8083=ORIENTED_EDGE('',*,*,#6223,.T.);
#8084=ORIENTED_EDGE('',*,*,#6255,.F.);
#8085=ORIENTED_EDGE('',*,*,#6230,.T.);
#8086=ORIENTED_EDGE('',*,*,#6238,.T.);
#8087=ORIENTED_EDGE('',*,*,#6234,.T.);
#8088=ORIENTED_EDGE('',*,*,#6252,.F.);
#8089=ORIENTED_EDGE('',*,*,#6267,.F.);
#8090=ORIENTED_EDGE('',*,*,#6268,.T.);
#8091=ORIENTED_EDGE('',*,*,#6261,.T.);
#8092=ORIENTED_EDGE('',*,*,#6266,.T.);
#8093=ORIENTED_EDGE('',*,*,#6264,.T.);
#8094=ORIENTED_EDGE('',*,*,#6269,.T.);
#8095=ORIENTED_EDGE('',*,*,#6270,.T.);
#8096=ORIENTED_EDGE('',*,*,#6253,.F.);
#8097=ORIENTED_EDGE('',*,*,#6219,.T.);
#8098=ORIENTED_EDGE('',*,*,#6227,.T.);
#8099=ORIENTED_EDGE('',*,*,#6263,.T.);
#8100=ORIENTED_EDGE('',*,*,#6243,.F.);
#8101=ORIENTED_EDGE('',*,*,#6271,.F.);
#8102=ORIENTED_EDGE('',*,*,#6269,.F.);
#8103=ORIENTED_EDGE('',*,*,#6256,.T.);
#8104=ORIENTED_EDGE('',*,*,#6262,.T.);
#8105=ORIENTED_EDGE('',*,*,#6268,.F.);
#8106=ORIENTED_EDGE('',*,*,#6272,.F.);
#8107=ORIENTED_EDGE('',*,*,#6247,.F.);
#8108=ORIENTED_EDGE('',*,*,#6258,.T.);
#8109=ORIENTED_EDGE('',*,*,#6272,.T.);
#8110=ORIENTED_EDGE('',*,*,#6267,.T.);
#8111=ORIENTED_EDGE('',*,*,#6251,.F.);
#8112=ORIENTED_EDGE('',*,*,#6248,.F.);
#8113=ORIENTED_EDGE('',*,*,#6271,.T.);
#8114=ORIENTED_EDGE('',*,*,#6242,.T.);
#8115=ORIENTED_EDGE('',*,*,#6254,.F.);
#8116=ORIENTED_EDGE('',*,*,#6270,.F.);
#8117=ORIENTED_EDGE('',*,*,#6273,.F.);
#8118=ORIENTED_EDGE('',*,*,#6274,.F.);
#8119=ORIENTED_EDGE('',*,*,#6275,.F.);
#8120=ORIENTED_EDGE('',*,*,#6276,.F.);
#8121=ORIENTED_EDGE('',*,*,#6277,.F.);
#8122=ORIENTED_EDGE('',*,*,#6278,.F.);
#8123=ORIENTED_EDGE('',*,*,#6279,.F.);
#8124=ORIENTED_EDGE('',*,*,#6280,.F.);
#8125=ORIENTED_EDGE('',*,*,#6281,.F.);
#8126=ORIENTED_EDGE('',*,*,#6276,.T.);
#8127=ORIENTED_EDGE('',*,*,#6282,.F.);
#8128=ORIENTED_EDGE('',*,*,#6278,.T.);
#8129=ORIENTED_EDGE('',*,*,#6283,.F.);
#8130=ORIENTED_EDGE('',*,*,#6284,.F.);
#8131=ORIENTED_EDGE('',*,*,#6285,.F.);
#8132=ORIENTED_EDGE('',*,*,#6286,.F.);
#8133=ORIENTED_EDGE('',*,*,#6287,.F.);
#8134=ORIENTED_EDGE('',*,*,#6288,.F.);
#8135=ORIENTED_EDGE('',*,*,#6289,.F.);
#8136=ORIENTED_EDGE('',*,*,#6290,.F.);
#8137=ORIENTED_EDGE('',*,*,#6291,.F.);
#8138=ORIENTED_EDGE('',*,*,#6292,.F.);
#8139=ORIENTED_EDGE('',*,*,#6287,.T.);
#8140=ORIENTED_EDGE('',*,*,#6293,.F.);
#8141=ORIENTED_EDGE('',*,*,#6289,.T.);
#8142=ORIENTED_EDGE('',*,*,#6294,.F.);
#8143=ORIENTED_EDGE('',*,*,#6279,.T.);
#8144=ORIENTED_EDGE('',*,*,#6282,.T.);
#8145=ORIENTED_EDGE('',*,*,#6275,.T.);
#8146=ORIENTED_EDGE('',*,*,#6295,.F.);
#8147=ORIENTED_EDGE('',*,*,#6296,.F.);
#8148=ORIENTED_EDGE('',*,*,#6297,.T.);
#8149=ORIENTED_EDGE('',*,*,#6298,.T.);
#8150=ORIENTED_EDGE('',*,*,#6299,.T.);
#8151=ORIENTED_EDGE('',*,*,#6300,.T.);
#8152=ORIENTED_EDGE('',*,*,#6301,.T.);
#8153=ORIENTED_EDGE('',*,*,#6302,.T.);
#8154=ORIENTED_EDGE('',*,*,#6303,.F.);
#8155=ORIENTED_EDGE('',*,*,#6290,.T.);
#8156=ORIENTED_EDGE('',*,*,#6293,.T.);
#8157=ORIENTED_EDGE('',*,*,#6286,.T.);
#8158=ORIENTED_EDGE('',*,*,#6304,.F.);
#8159=ORIENTED_EDGE('',*,*,#6291,.T.);
#8160=ORIENTED_EDGE('',*,*,#6303,.T.);
#8161=ORIENTED_EDGE('',*,*,#6305,.T.);
#8162=ORIENTED_EDGE('',*,*,#6306,.T.);
#8163=ORIENTED_EDGE('',*,*,#6274,.T.);
#8164=ORIENTED_EDGE('',*,*,#6307,.T.);
#8165=ORIENTED_EDGE('',*,*,#6308,.T.);
#8166=ORIENTED_EDGE('',*,*,#6295,.T.);
#8167=ORIENTED_EDGE('',*,*,#6280,.T.);
#8168=ORIENTED_EDGE('',*,*,#6304,.T.);
#8169=ORIENTED_EDGE('',*,*,#6285,.T.);
#8170=ORIENTED_EDGE('',*,*,#6309,.T.);
#8171=ORIENTED_EDGE('',*,*,#6310,.F.);
#8172=ORIENTED_EDGE('',*,*,#6311,.T.);
#8173=ORIENTED_EDGE('',*,*,#6283,.T.);
#8174=ORIENTED_EDGE('',*,*,#6311,.F.);
#8175=ORIENTED_EDGE('',*,*,#6312,.F.);
#8176=ORIENTED_EDGE('',*,*,#6313,.T.);
#8177=ORIENTED_EDGE('',*,*,#6294,.T.);
#8178=ORIENTED_EDGE('',*,*,#6313,.F.);
#8179=ORIENTED_EDGE('',*,*,#6300,.F.);
#8180=ORIENTED_EDGE('',*,*,#6314,.T.);
#8181=ORIENTED_EDGE('',*,*,#6315,.F.);
#8182=ORIENTED_EDGE('',*,*,#6316,.F.);
#8183=ORIENTED_EDGE('',*,*,#6298,.F.);
#8184=ORIENTED_EDGE('',*,*,#6317,.F.);
#8185=ORIENTED_EDGE('',*,*,#6318,.F.);
#8186=ORIENTED_EDGE('',*,*,#6319,.T.);
#8187=ORIENTED_EDGE('',*,*,#6299,.F.);
#8188=ORIENTED_EDGE('',*,*,#6319,.F.);
#8189=ORIENTED_EDGE('',*,*,#6320,.F.);
#8190=ORIENTED_EDGE('',*,*,#6314,.F.);
#8191=ORIENTED_EDGE('',*,*,#6277,.T.);
#8192=ORIENTED_EDGE('',*,*,#6309,.F.);
#8193=ORIENTED_EDGE('',*,*,#6284,.T.);
#8194=ORIENTED_EDGE('',*,*,#6292,.T.);
#8195=ORIENTED_EDGE('',*,*,#6288,.T.);
#8196=ORIENTED_EDGE('',*,*,#6306,.F.);
#8197=ORIENTED_EDGE('',*,*,#6321,.F.);
#8198=ORIENTED_EDGE('',*,*,#6322,.T.);
#8199=ORIENTED_EDGE('',*,*,#6315,.T.);
#8200=ORIENTED_EDGE('',*,*,#6320,.T.);
#8201=ORIENTED_EDGE('',*,*,#6318,.T.);
#8202=ORIENTED_EDGE('',*,*,#6323,.T.);
#8203=ORIENTED_EDGE('',*,*,#6324,.T.);
#8204=ORIENTED_EDGE('',*,*,#6307,.F.);
#8205=ORIENTED_EDGE('',*,*,#6273,.T.);
#8206=ORIENTED_EDGE('',*,*,#6281,.T.);
#8207=ORIENTED_EDGE('',*,*,#6317,.T.);
#8208=ORIENTED_EDGE('',*,*,#6297,.F.);
#8209=ORIENTED_EDGE('',*,*,#6325,.F.);
#8210=ORIENTED_EDGE('',*,*,#6323,.F.);
#8211=ORIENTED_EDGE('',*,*,#6310,.T.);
#8212=ORIENTED_EDGE('',*,*,#6316,.T.);
#8213=ORIENTED_EDGE('',*,*,#6322,.F.);
#8214=ORIENTED_EDGE('',*,*,#6326,.F.);
#8215=ORIENTED_EDGE('',*,*,#6301,.F.);
#8216=ORIENTED_EDGE('',*,*,#6312,.T.);
#8217=ORIENTED_EDGE('',*,*,#6326,.T.);
#8218=ORIENTED_EDGE('',*,*,#6321,.T.);
#8219=ORIENTED_EDGE('',*,*,#6305,.F.);
#8220=ORIENTED_EDGE('',*,*,#6302,.F.);
#8221=ORIENTED_EDGE('',*,*,#6325,.T.);
#8222=ORIENTED_EDGE('',*,*,#6296,.T.);
#8223=ORIENTED_EDGE('',*,*,#6308,.F.);
#8224=ORIENTED_EDGE('',*,*,#6324,.F.);
#8225=ORIENTED_EDGE('',*,*,#6327,.F.);
#8226=ORIENTED_EDGE('',*,*,#6328,.F.);
#8227=ORIENTED_EDGE('',*,*,#6329,.T.);
#8228=ORIENTED_EDGE('',*,*,#6330,.F.);
#8229=ORIENTED_EDGE('',*,*,#6331,.F.);
#8230=ORIENTED_EDGE('',*,*,#6329,.F.);
#8231=ORIENTED_EDGE('',*,*,#6330,.T.);
#8232=ORIENTED_EDGE('',*,*,#6331,.T.);
#8233=ORIENTED_EDGE('',*,*,#6332,.T.);
#8234=ORIENTED_EDGE('',*,*,#6333,.T.);
#8235=ORIENTED_EDGE('',*,*,#6332,.F.);
#8236=ORIENTED_EDGE('',*,*,#6334,.T.);
#8237=ORIENTED_EDGE('',*,*,#6335,.T.);
#8238=ORIENTED_EDGE('',*,*,#6336,.F.);
#8239=ORIENTED_EDGE('',*,*,#6335,.F.);
#8240=ORIENTED_EDGE('',*,*,#6336,.T.);
#8241=ORIENTED_EDGE('',*,*,#6337,.T.);
#8242=ORIENTED_EDGE('',*,*,#6338,.F.);
#8243=ORIENTED_EDGE('',*,*,#6337,.F.);
#8244=ORIENTED_EDGE('',*,*,#6333,.F.);
#8245=ORIENTED_EDGE('',*,*,#6338,.T.);
#8246=ORIENTED_EDGE('',*,*,#6339,.F.);
#8247=ORIENTED_EDGE('',*,*,#6340,.T.);
#8248=ORIENTED_EDGE('',*,*,#6327,.T.);
#8249=ORIENTED_EDGE('',*,*,#6328,.T.);
#8250=ORIENTED_EDGE('',*,*,#6340,.F.);
#8251=ORIENTED_EDGE('',*,*,#6339,.T.);
#8252=ORIENTED_EDGE('',*,*,#6341,.F.);
#8253=ORIENTED_EDGE('',*,*,#6341,.T.);
#8254=ORIENTED_EDGE('',*,*,#6342,.T.);
#8255=ORIENTED_EDGE('',*,*,#6334,.F.);
#8256=ORIENTED_EDGE('',*,*,#6342,.F.);
#8257=ORIENTED_EDGE('',*,*,#6343,.F.);
#8258=ORIENTED_EDGE('',*,*,#6344,.F.);
#8259=ORIENTED_EDGE('',*,*,#6345,.T.);
#8260=ORIENTED_EDGE('',*,*,#6346,.F.);
#8261=ORIENTED_EDGE('',*,*,#6347,.F.);
#8262=ORIENTED_EDGE('',*,*,#6345,.F.);
#8263=ORIENTED_EDGE('',*,*,#6348,.T.);
#8264=ORIENTED_EDGE('',*,*,#6349,.T.);
#8265=ORIENTED_EDGE('',*,*,#6346,.T.);
#8266=ORIENTED_EDGE('',*,*,#6347,.T.);
#8267=ORIENTED_EDGE('',*,*,#6349,.F.);
#8268=ORIENTED_EDGE('',*,*,#6350,.F.);
#8269=ORIENTED_EDGE('',*,*,#6351,.T.);
#8270=ORIENTED_EDGE('',*,*,#6352,.F.);
#8271=ORIENTED_EDGE('',*,*,#6353,.T.);
#8272=ORIENTED_EDGE('',*,*,#6350,.T.);
#8273=ORIENTED_EDGE('',*,*,#6353,.F.);
#8274=ORIENTED_EDGE('',*,*,#6354,.F.);
#8275=ORIENTED_EDGE('',*,*,#6355,.T.);
#8276=ORIENTED_EDGE('',*,*,#6352,.T.);
#8277=ORIENTED_EDGE('',*,*,#6355,.F.);
#8278=ORIENTED_EDGE('',*,*,#6356,.F.);
#8279=ORIENTED_EDGE('',*,*,#6357,.T.);
#8280=ORIENTED_EDGE('',*,*,#6354,.T.);
#8281=ORIENTED_EDGE('',*,*,#6357,.F.);
#8282=ORIENTED_EDGE('',*,*,#6356,.T.);
#8283=ORIENTED_EDGE('',*,*,#6348,.F.);
#8284=ORIENTED_EDGE('',*,*,#6343,.T.);
#8285=ORIENTED_EDGE('',*,*,#6344,.T.);
#8286=ORIENTED_EDGE('',*,*,#6358,.T.);
#8287=ORIENTED_EDGE('',*,*,#6351,.F.);
#8288=ORIENTED_EDGE('',*,*,#6358,.F.);
#8289=ORIENTED_EDGE('',*,*,#6359,.T.);
#8290=ORIENTED_EDGE('',*,*,#6359,.F.);
#8291=ORIENTED_EDGE('',*,*,#6360,.T.);
#8292=ORIENTED_EDGE('',*,*,#6360,.F.);
#8293=ORIENTED_EDGE('',*,*,#6361,.T.);
#8294=ORIENTED_EDGE('',*,*,#6361,.F.);
#8295=ORIENTED_EDGE('',*,*,#6362,.T.);
#8296=ORIENTED_EDGE('',*,*,#6362,.F.);
#8297=ORIENTED_EDGE('',*,*,#6363,.T.);
#8298=ORIENTED_EDGE('',*,*,#6363,.F.);
#8299=ORIENTED_EDGE('',*,*,#6364,.T.);
#8300=ORIENTED_EDGE('',*,*,#6364,.F.);
#8301=ORIENTED_EDGE('',*,*,#6365,.T.);
#8302=ORIENTED_EDGE('',*,*,#6365,.F.);
#8303=ORIENTED_EDGE('',*,*,#6366,.T.);
#8304=ORIENTED_EDGE('',*,*,#6366,.F.);
#8305=ORIENTED_EDGE('',*,*,#6367,.F.);
#8306=ORIENTED_EDGE('',*,*,#6368,.F.);
#8307=ORIENTED_EDGE('',*,*,#6369,.F.);
#8308=ORIENTED_EDGE('',*,*,#6370,.F.);
#8309=ORIENTED_EDGE('',*,*,#6369,.T.);
#8310=ORIENTED_EDGE('',*,*,#6371,.F.);
#8311=ORIENTED_EDGE('',*,*,#6372,.T.);
#8312=ORIENTED_EDGE('',*,*,#6373,.F.);
#8313=ORIENTED_EDGE('',*,*,#6374,.T.);
#8314=ORIENTED_EDGE('',*,*,#6375,.F.);
#8315=ORIENTED_EDGE('',*,*,#6376,.T.);
#8316=ORIENTED_EDGE('',*,*,#6377,.T.);
#8317=ORIENTED_EDGE('',*,*,#6378,.F.);
#8318=ORIENTED_EDGE('',*,*,#6377,.F.);
#8319=ORIENTED_EDGE('',*,*,#6379,.T.);
#8320=ORIENTED_EDGE('',*,*,#6380,.F.);
#8321=ORIENTED_EDGE('',*,*,#6381,.T.);
#8322=ORIENTED_EDGE('',*,*,#6382,.F.);
#8323=ORIENTED_EDGE('',*,*,#6383,.T.);
#8324=ORIENTED_EDGE('',*,*,#6384,.F.);
#8325=ORIENTED_EDGE('',*,*,#6385,.T.);
#8326=ORIENTED_EDGE('',*,*,#6386,.F.);
#8327=ORIENTED_EDGE('',*,*,#6387,.T.);
#8328=ORIENTED_EDGE('',*,*,#6388,.F.);
#8329=ORIENTED_EDGE('',*,*,#6368,.T.);
#8330=ORIENTED_EDGE('',*,*,#6389,.T.);
#8331=ORIENTED_EDGE('',*,*,#6390,.T.);
#8332=ORIENTED_EDGE('',*,*,#6371,.T.);
#8333=ORIENTED_EDGE('',*,*,#6391,.F.);
#8334=ORIENTED_EDGE('',*,*,#6392,.F.);
#8335=ORIENTED_EDGE('',*,*,#6372,.F.);
#8336=ORIENTED_EDGE('',*,*,#6390,.F.);
#8337=ORIENTED_EDGE('',*,*,#6392,.T.);
#8338=ORIENTED_EDGE('',*,*,#6393,.T.);
#8339=ORIENTED_EDGE('',*,*,#6394,.T.);
#8340=ORIENTED_EDGE('',*,*,#6373,.T.);
#8341=ORIENTED_EDGE('',*,*,#6395,.F.);
#8342=ORIENTED_EDGE('',*,*,#6396,.F.);
#8343=ORIENTED_EDGE('',*,*,#6374,.F.);
#8344=ORIENTED_EDGE('',*,*,#6394,.F.);
#8345=ORIENTED_EDGE('',*,*,#6396,.T.);
#8346=ORIENTED_EDGE('',*,*,#6397,.T.);
#8347=ORIENTED_EDGE('',*,*,#6398,.T.);
#8348=ORIENTED_EDGE('',*,*,#6375,.T.);
#8349=ORIENTED_EDGE('',*,*,#6399,.F.);
#8350=ORIENTED_EDGE('',*,*,#6400,.F.);
#8351=ORIENTED_EDGE('',*,*,#6379,.F.);
#8352=ORIENTED_EDGE('',*,*,#6376,.F.);
#8353=ORIENTED_EDGE('',*,*,#6398,.F.);
#8354=ORIENTED_EDGE('',*,*,#6401,.F.);
#8355=ORIENTED_EDGE('',*,*,#6400,.T.);
#8356=ORIENTED_EDGE('',*,*,#6402,.T.);
#8357=ORIENTED_EDGE('',*,*,#6403,.T.);
#8358=ORIENTED_EDGE('',*,*,#6380,.T.);
#8359=ORIENTED_EDGE('',*,*,#6404,.F.);
#8360=ORIENTED_EDGE('',*,*,#6405,.F.);
#8361=ORIENTED_EDGE('',*,*,#6381,.F.);
#8362=ORIENTED_EDGE('',*,*,#6403,.F.);
#8363=ORIENTED_EDGE('',*,*,#6405,.T.);
#8364=ORIENTED_EDGE('',*,*,#6406,.T.);
#8365=ORIENTED_EDGE('',*,*,#6407,.T.);
#8366=ORIENTED_EDGE('',*,*,#6382,.T.);
#8367=ORIENTED_EDGE('',*,*,#6408,.F.);
#8368=ORIENTED_EDGE('',*,*,#6409,.F.);
#8369=ORIENTED_EDGE('',*,*,#6383,.F.);
#8370=ORIENTED_EDGE('',*,*,#6407,.F.);
#8371=ORIENTED_EDGE('',*,*,#6409,.T.);
#8372=ORIENTED_EDGE('',*,*,#6410,.T.);
#8373=ORIENTED_EDGE('',*,*,#6411,.T.);
#8374=ORIENTED_EDGE('',*,*,#6384,.T.);
#8375=ORIENTED_EDGE('',*,*,#6385,.F.);
#8376=ORIENTED_EDGE('',*,*,#6411,.F.);
#8377=ORIENTED_EDGE('',*,*,#6412,.F.);
#8378=ORIENTED_EDGE('',*,*,#6413,.F.);
#8379=ORIENTED_EDGE('',*,*,#6414,.F.);
#8380=ORIENTED_EDGE('',*,*,#6415,.T.);
#8381=ORIENTED_EDGE('',*,*,#6401,.T.);
#8382=ORIENTED_EDGE('',*,*,#6397,.F.);
#8383=ORIENTED_EDGE('',*,*,#6395,.T.);
#8384=ORIENTED_EDGE('',*,*,#6393,.F.);
#8385=ORIENTED_EDGE('',*,*,#6391,.T.);
#8386=ORIENTED_EDGE('',*,*,#6389,.F.);
#8387=ORIENTED_EDGE('',*,*,#6367,.T.);
#8388=ORIENTED_EDGE('',*,*,#6416,.F.);
#8389=ORIENTED_EDGE('',*,*,#6417,.T.);
#8390=ORIENTED_EDGE('',*,*,#6418,.F.);
#8391=ORIENTED_EDGE('',*,*,#6412,.T.);
#8392=ORIENTED_EDGE('',*,*,#6410,.F.);
#8393=ORIENTED_EDGE('',*,*,#6408,.T.);
#8394=ORIENTED_EDGE('',*,*,#6406,.F.);
#8395=ORIENTED_EDGE('',*,*,#6404,.T.);
#8396=ORIENTED_EDGE('',*,*,#6402,.F.);
#8397=ORIENTED_EDGE('',*,*,#6399,.T.);
#8398=ORIENTED_EDGE('',*,*,#6415,.F.);
#8399=ORIENTED_EDGE('',*,*,#6370,.T.);
#8400=ORIENTED_EDGE('',*,*,#6388,.T.);
#8401=ORIENTED_EDGE('',*,*,#6419,.T.);
#8402=ORIENTED_EDGE('',*,*,#6416,.T.);
#8403=ORIENTED_EDGE('',*,*,#6387,.F.);
#8404=ORIENTED_EDGE('',*,*,#6420,.F.);
#8405=ORIENTED_EDGE('',*,*,#6417,.F.);
#8406=ORIENTED_EDGE('',*,*,#6419,.F.);
#8407=ORIENTED_EDGE('',*,*,#6378,.T.);
#8408=ORIENTED_EDGE('',*,*,#6414,.T.);
#8409=ORIENTED_EDGE('',*,*,#6413,.T.);
#8410=ORIENTED_EDGE('',*,*,#6418,.T.);
#8411=ORIENTED_EDGE('',*,*,#6420,.T.);
#8412=ORIENTED_EDGE('',*,*,#6386,.T.);
#8413=ORIENTED_EDGE('',*,*,#6421,.F.);
#8414=ORIENTED_EDGE('',*,*,#6422,.T.);
#8415=ORIENTED_EDGE('',*,*,#6423,.F.);
#8416=ORIENTED_EDGE('',*,*,#6424,.T.);
#8417=ORIENTED_EDGE('',*,*,#6421,.T.);
#8418=ORIENTED_EDGE('',*,*,#6424,.F.);
#8419=ORIENTED_EDGE('',*,*,#6423,.T.);
#8420=ORIENTED_EDGE('',*,*,#6425,.F.);
#8421=ORIENTED_EDGE('',*,*,#6425,.T.);
#8422=ORIENTED_EDGE('',*,*,#6426,.T.);
#8423=ORIENTED_EDGE('',*,*,#6422,.F.);
#8424=ORIENTED_EDGE('',*,*,#6426,.F.);
#8425=ORIENTED_EDGE('',*,*,#6427,.F.);
#8426=ORIENTED_EDGE('',*,*,#6428,.T.);
#8427=ORIENTED_EDGE('',*,*,#6429,.F.);
#8428=ORIENTED_EDGE('',*,*,#6430,.T.);
#8429=ORIENTED_EDGE('',*,*,#6427,.T.);
#8430=ORIENTED_EDGE('',*,*,#6430,.F.);
#8431=ORIENTED_EDGE('',*,*,#6429,.T.);
#8432=ORIENTED_EDGE('',*,*,#6431,.F.);
#8433=ORIENTED_EDGE('',*,*,#6431,.T.);
#8434=ORIENTED_EDGE('',*,*,#6432,.T.);
#8435=ORIENTED_EDGE('',*,*,#6428,.F.);
#8436=ORIENTED_EDGE('',*,*,#6432,.F.);
#8437=ORIENTED_EDGE('',*,*,#6433,.F.);
#8438=ORIENTED_EDGE('',*,*,#6434,.T.);
#8439=ORIENTED_EDGE('',*,*,#6435,.F.);
#8440=ORIENTED_EDGE('',*,*,#6436,.F.);
#8441=ORIENTED_EDGE('',*,*,#6437,.F.);
#8442=ORIENTED_EDGE('',*,*,#6438,.T.);
#8443=ORIENTED_EDGE('',*,*,#6439,.F.);
#8444=ORIENTED_EDGE('',*,*,#6434,.F.);
#8445=ORIENTED_EDGE('',*,*,#6440,.F.);
#8446=ORIENTED_EDGE('',*,*,#6441,.T.);
#8447=ORIENTED_EDGE('',*,*,#6442,.F.);
#8448=ORIENTED_EDGE('',*,*,#6438,.F.);
#8449=ORIENTED_EDGE('',*,*,#6443,.F.);
#8450=ORIENTED_EDGE('',*,*,#6444,.T.);
#8451=ORIENTED_EDGE('',*,*,#6445,.F.);
#8452=ORIENTED_EDGE('',*,*,#6441,.F.);
#8453=ORIENTED_EDGE('',*,*,#6446,.F.);
#8454=ORIENTED_EDGE('',*,*,#6447,.T.);
#8455=ORIENTED_EDGE('',*,*,#6448,.F.);
#8456=ORIENTED_EDGE('',*,*,#6444,.F.);
#8457=ORIENTED_EDGE('',*,*,#6449,.F.);
#8458=ORIENTED_EDGE('',*,*,#6450,.T.);
#8459=ORIENTED_EDGE('',*,*,#6451,.F.);
#8460=ORIENTED_EDGE('',*,*,#6447,.F.);
#8461=ORIENTED_EDGE('',*,*,#6452,.F.);
#8462=ORIENTED_EDGE('',*,*,#6453,.T.);
#8463=ORIENTED_EDGE('',*,*,#6454,.F.);
#8464=ORIENTED_EDGE('',*,*,#6450,.F.);
#8465=ORIENTED_EDGE('',*,*,#6455,.F.);
#8466=ORIENTED_EDGE('',*,*,#6456,.T.);
#8467=ORIENTED_EDGE('',*,*,#6457,.F.);
#8468=ORIENTED_EDGE('',*,*,#6453,.F.);
#8469=ORIENTED_EDGE('',*,*,#6458,.F.);
#8470=ORIENTED_EDGE('',*,*,#6459,.F.);
#8471=ORIENTED_EDGE('',*,*,#6460,.F.);
#8472=ORIENTED_EDGE('',*,*,#6456,.F.);
#8473=ORIENTED_EDGE('',*,*,#6461,.F.);
#8474=ORIENTED_EDGE('',*,*,#6462,.T.);
#8475=ORIENTED_EDGE('',*,*,#6463,.F.);
#8476=ORIENTED_EDGE('',*,*,#6464,.F.);
#8477=ORIENTED_EDGE('',*,*,#6465,.F.);
#8478=ORIENTED_EDGE('',*,*,#6466,.T.);
#8479=ORIENTED_EDGE('',*,*,#6467,.F.);
#8480=ORIENTED_EDGE('',*,*,#6462,.F.);
#8481=ORIENTED_EDGE('',*,*,#6468,.F.);
#8482=ORIENTED_EDGE('',*,*,#6469,.T.);
#8483=ORIENTED_EDGE('',*,*,#6470,.F.);
#8484=ORIENTED_EDGE('',*,*,#6466,.F.);
#8485=ORIENTED_EDGE('',*,*,#6471,.F.);
#8486=ORIENTED_EDGE('',*,*,#6472,.T.);
#8487=ORIENTED_EDGE('',*,*,#6473,.F.);
#8488=ORIENTED_EDGE('',*,*,#6469,.F.);
#8489=ORIENTED_EDGE('',*,*,#6474,.F.);
#8490=ORIENTED_EDGE('',*,*,#6475,.T.);
#8491=ORIENTED_EDGE('',*,*,#6476,.F.);
#8492=ORIENTED_EDGE('',*,*,#6472,.F.);
#8493=ORIENTED_EDGE('',*,*,#6477,.F.);
#8494=ORIENTED_EDGE('',*,*,#6478,.T.);
#8495=ORIENTED_EDGE('',*,*,#6479,.F.);
#8496=ORIENTED_EDGE('',*,*,#6475,.F.);
#8497=ORIENTED_EDGE('',*,*,#6480,.F.);
#8498=ORIENTED_EDGE('',*,*,#6481,.T.);
#8499=ORIENTED_EDGE('',*,*,#6482,.F.);
#8500=ORIENTED_EDGE('',*,*,#6478,.F.);
#8501=ORIENTED_EDGE('',*,*,#6483,.F.);
#8502=ORIENTED_EDGE('',*,*,#6484,.T.);
#8503=ORIENTED_EDGE('',*,*,#6485,.F.);
#8504=ORIENTED_EDGE('',*,*,#6481,.F.);
#8505=ORIENTED_EDGE('',*,*,#6486,.F.);
#8506=ORIENTED_EDGE('',*,*,#6487,.F.);
#8507=ORIENTED_EDGE('',*,*,#6488,.F.);
#8508=ORIENTED_EDGE('',*,*,#6484,.F.);
#8509=ORIENTED_EDGE('',*,*,#6489,.F.);
#8510=ORIENTED_EDGE('',*,*,#6490,.T.);
#8511=ORIENTED_EDGE('',*,*,#6491,.F.);
#8512=ORIENTED_EDGE('',*,*,#6492,.F.);
#8513=ORIENTED_EDGE('',*,*,#6493,.F.);
#8514=ORIENTED_EDGE('',*,*,#6494,.T.);
#8515=ORIENTED_EDGE('',*,*,#6495,.F.);
#8516=ORIENTED_EDGE('',*,*,#6490,.F.);
#8517=ORIENTED_EDGE('',*,*,#6496,.F.);
#8518=ORIENTED_EDGE('',*,*,#6497,.T.);
#8519=ORIENTED_EDGE('',*,*,#6498,.F.);
#8520=ORIENTED_EDGE('',*,*,#6494,.F.);
#8521=ORIENTED_EDGE('',*,*,#6499,.F.);
#8522=ORIENTED_EDGE('',*,*,#6500,.T.);
#8523=ORIENTED_EDGE('',*,*,#6501,.F.);
#8524=ORIENTED_EDGE('',*,*,#6497,.F.);
#8525=ORIENTED_EDGE('',*,*,#6502,.F.);
#8526=ORIENTED_EDGE('',*,*,#6503,.T.);
#8527=ORIENTED_EDGE('',*,*,#6504,.F.);
#8528=ORIENTED_EDGE('',*,*,#6500,.F.);
#8529=ORIENTED_EDGE('',*,*,#6505,.F.);
#8530=ORIENTED_EDGE('',*,*,#6506,.T.);
#8531=ORIENTED_EDGE('',*,*,#6507,.F.);
#8532=ORIENTED_EDGE('',*,*,#6503,.F.);
#8533=ORIENTED_EDGE('',*,*,#6508,.F.);
#8534=ORIENTED_EDGE('',*,*,#6509,.T.);
#8535=ORIENTED_EDGE('',*,*,#6510,.F.);
#8536=ORIENTED_EDGE('',*,*,#6506,.F.);
#8537=ORIENTED_EDGE('',*,*,#6511,.F.);
#8538=ORIENTED_EDGE('',*,*,#6512,.T.);
#8539=ORIENTED_EDGE('',*,*,#6513,.F.);
#8540=ORIENTED_EDGE('',*,*,#6509,.F.);
#8541=ORIENTED_EDGE('',*,*,#6514,.F.);
#8542=ORIENTED_EDGE('',*,*,#6515,.F.);
#8543=ORIENTED_EDGE('',*,*,#6516,.F.);
#8544=ORIENTED_EDGE('',*,*,#6512,.F.);
#8545=ORIENTED_EDGE('',*,*,#6517,.F.);
#8546=ORIENTED_EDGE('',*,*,#6518,.T.);
#8547=ORIENTED_EDGE('',*,*,#6519,.F.);
#8548=ORIENTED_EDGE('',*,*,#6520,.F.);
#8549=ORIENTED_EDGE('',*,*,#6521,.F.);
#8550=ORIENTED_EDGE('',*,*,#6522,.T.);
#8551=ORIENTED_EDGE('',*,*,#6523,.F.);
#8552=ORIENTED_EDGE('',*,*,#6518,.F.);
#8553=ORIENTED_EDGE('',*,*,#6524,.F.);
#8554=ORIENTED_EDGE('',*,*,#6525,.T.);
#8555=ORIENTED_EDGE('',*,*,#6526,.F.);
#8556=ORIENTED_EDGE('',*,*,#6522,.F.);
#8557=ORIENTED_EDGE('',*,*,#6527,.F.);
#8558=ORIENTED_EDGE('',*,*,#6528,.T.);
#8559=ORIENTED_EDGE('',*,*,#6529,.F.);
#8560=ORIENTED_EDGE('',*,*,#6525,.F.);
#8561=ORIENTED_EDGE('',*,*,#6530,.F.);
#8562=ORIENTED_EDGE('',*,*,#6531,.T.);
#8563=ORIENTED_EDGE('',*,*,#6532,.F.);
#8564=ORIENTED_EDGE('',*,*,#6528,.F.);
#8565=ORIENTED_EDGE('',*,*,#6533,.F.);
#8566=ORIENTED_EDGE('',*,*,#6534,.T.);
#8567=ORIENTED_EDGE('',*,*,#6535,.F.);
#8568=ORIENTED_EDGE('',*,*,#6531,.F.);
#8569=ORIENTED_EDGE('',*,*,#6536,.F.);
#8570=ORIENTED_EDGE('',*,*,#6537,.T.);
#8571=ORIENTED_EDGE('',*,*,#6538,.F.);
#8572=ORIENTED_EDGE('',*,*,#6534,.F.);
#8573=ORIENTED_EDGE('',*,*,#6539,.F.);
#8574=ORIENTED_EDGE('',*,*,#6540,.T.);
#8575=ORIENTED_EDGE('',*,*,#6541,.F.);
#8576=ORIENTED_EDGE('',*,*,#6537,.F.);
#8577=ORIENTED_EDGE('',*,*,#6542,.F.);
#8578=ORIENTED_EDGE('',*,*,#6543,.F.);
#8579=ORIENTED_EDGE('',*,*,#6544,.F.);
#8580=ORIENTED_EDGE('',*,*,#6540,.F.);
#8581=ORIENTED_EDGE('',*,*,#6545,.F.);
#8582=ORIENTED_EDGE('',*,*,#6546,.T.);
#8583=ORIENTED_EDGE('',*,*,#6547,.F.);
#8584=ORIENTED_EDGE('',*,*,#6546,.F.);
#8585=ORIENTED_EDGE('',*,*,#6459,.T.);
#8586=ORIENTED_EDGE('',*,*,#6548,.T.);
#8587=ORIENTED_EDGE('',*,*,#6549,.T.);
#8588=ORIENTED_EDGE('',*,*,#6550,.F.);
#8589=ORIENTED_EDGE('',*,*,#6436,.T.);
#8590=ORIENTED_EDGE('',*,*,#6551,.F.);
#8591=ORIENTED_EDGE('',*,*,#6552,.F.);
#8592=ORIENTED_EDGE('',*,*,#6553,.T.);
#8593=ORIENTED_EDGE('',*,*,#6487,.T.);
#8594=ORIENTED_EDGE('',*,*,#6554,.T.);
#8595=ORIENTED_EDGE('',*,*,#6552,.T.);
#8596=ORIENTED_EDGE('',*,*,#6555,.F.);
#8597=ORIENTED_EDGE('',*,*,#6464,.T.);
#8598=ORIENTED_EDGE('',*,*,#6556,.F.);
#8599=ORIENTED_EDGE('',*,*,#6557,.F.);
#8600=ORIENTED_EDGE('',*,*,#6558,.T.);
#8601=ORIENTED_EDGE('',*,*,#6515,.T.);
#8602=ORIENTED_EDGE('',*,*,#6559,.T.);
#8603=ORIENTED_EDGE('',*,*,#6557,.T.);
#8604=ORIENTED_EDGE('',*,*,#6560,.F.);
#8605=ORIENTED_EDGE('',*,*,#6492,.T.);
#8606=ORIENTED_EDGE('',*,*,#6561,.F.);
#8607=ORIENTED_EDGE('',*,*,#6562,.F.);
#8608=ORIENTED_EDGE('',*,*,#6563,.T.);
#8609=ORIENTED_EDGE('',*,*,#6543,.T.);
#8610=ORIENTED_EDGE('',*,*,#6564,.T.);
#8611=ORIENTED_EDGE('',*,*,#6562,.T.);
#8612=ORIENTED_EDGE('',*,*,#6565,.F.);
#8613=ORIENTED_EDGE('',*,*,#6520,.T.);
#8614=ORIENTED_EDGE('',*,*,#6566,.F.);
#8615=ORIENTED_EDGE('',*,*,#6549,.F.);
#8616=ORIENTED_EDGE('',*,*,#6567,.T.);
#8617=ORIENTED_EDGE('',*,*,#6435,.T.);
#8618=ORIENTED_EDGE('',*,*,#6439,.T.);
#8619=ORIENTED_EDGE('',*,*,#6442,.T.);
#8620=ORIENTED_EDGE('',*,*,#6445,.T.);
#8621=ORIENTED_EDGE('',*,*,#6448,.T.);
#8622=ORIENTED_EDGE('',*,*,#6451,.T.);
#8623=ORIENTED_EDGE('',*,*,#6454,.T.);
#8624=ORIENTED_EDGE('',*,*,#6457,.T.);
#8625=ORIENTED_EDGE('',*,*,#6460,.T.);
#8626=ORIENTED_EDGE('',*,*,#6550,.T.);
#8627=ORIENTED_EDGE('',*,*,#6566,.T.);
#8628=ORIENTED_EDGE('',*,*,#6519,.T.);
#8629=ORIENTED_EDGE('',*,*,#6523,.T.);
#8630=ORIENTED_EDGE('',*,*,#6526,.T.);
#8631=ORIENTED_EDGE('',*,*,#6529,.T.);
#8632=ORIENTED_EDGE('',*,*,#6532,.T.);
#8633=ORIENTED_EDGE('',*,*,#6535,.T.);
#8634=ORIENTED_EDGE('',*,*,#6538,.T.);
#8635=ORIENTED_EDGE('',*,*,#6541,.T.);
#8636=ORIENTED_EDGE('',*,*,#6544,.T.);
#8637=ORIENTED_EDGE('',*,*,#6565,.T.);
#8638=ORIENTED_EDGE('',*,*,#6561,.T.);
#8639=ORIENTED_EDGE('',*,*,#6491,.T.);
#8640=ORIENTED_EDGE('',*,*,#6495,.T.);
#8641=ORIENTED_EDGE('',*,*,#6498,.T.);
#8642=ORIENTED_EDGE('',*,*,#6501,.T.);
#8643=ORIENTED_EDGE('',*,*,#6504,.T.);
#8644=ORIENTED_EDGE('',*,*,#6507,.T.);
#8645=ORIENTED_EDGE('',*,*,#6510,.T.);
#8646=ORIENTED_EDGE('',*,*,#6513,.T.);
#8647=ORIENTED_EDGE('',*,*,#6516,.T.);
#8648=ORIENTED_EDGE('',*,*,#6560,.T.);
#8649=ORIENTED_EDGE('',*,*,#6556,.T.);
#8650=ORIENTED_EDGE('',*,*,#6463,.T.);
#8651=ORIENTED_EDGE('',*,*,#6467,.T.);
#8652=ORIENTED_EDGE('',*,*,#6470,.T.);
#8653=ORIENTED_EDGE('',*,*,#6473,.T.);
#8654=ORIENTED_EDGE('',*,*,#6476,.T.);
#8655=ORIENTED_EDGE('',*,*,#6479,.T.);
#8656=ORIENTED_EDGE('',*,*,#6482,.T.);
#8657=ORIENTED_EDGE('',*,*,#6485,.T.);
#8658=ORIENTED_EDGE('',*,*,#6488,.T.);
#8659=ORIENTED_EDGE('',*,*,#6555,.T.);
#8660=ORIENTED_EDGE('',*,*,#6551,.T.);
#8661=ORIENTED_EDGE('',*,*,#6547,.T.);
#8662=ORIENTED_EDGE('',*,*,#6433,.T.);
#8663=ORIENTED_EDGE('',*,*,#6553,.F.);
#8664=ORIENTED_EDGE('',*,*,#6554,.F.);
#8665=ORIENTED_EDGE('',*,*,#6486,.T.);
#8666=ORIENTED_EDGE('',*,*,#6483,.T.);
#8667=ORIENTED_EDGE('',*,*,#6480,.T.);
#8668=ORIENTED_EDGE('',*,*,#6477,.T.);
#8669=ORIENTED_EDGE('',*,*,#6474,.T.);
#8670=ORIENTED_EDGE('',*,*,#6471,.T.);
#8671=ORIENTED_EDGE('',*,*,#6468,.T.);
#8672=ORIENTED_EDGE('',*,*,#6465,.T.);
#8673=ORIENTED_EDGE('',*,*,#6461,.T.);
#8674=ORIENTED_EDGE('',*,*,#6558,.F.);
#8675=ORIENTED_EDGE('',*,*,#6559,.F.);
#8676=ORIENTED_EDGE('',*,*,#6514,.T.);
#8677=ORIENTED_EDGE('',*,*,#6511,.T.);
#8678=ORIENTED_EDGE('',*,*,#6508,.T.);
#8679=ORIENTED_EDGE('',*,*,#6505,.T.);
#8680=ORIENTED_EDGE('',*,*,#6502,.T.);
#8681=ORIENTED_EDGE('',*,*,#6499,.T.);
#8682=ORIENTED_EDGE('',*,*,#6496,.T.);
#8683=ORIENTED_EDGE('',*,*,#6493,.T.);
#8684=ORIENTED_EDGE('',*,*,#6489,.T.);
#8685=ORIENTED_EDGE('',*,*,#6563,.F.);
#8686=ORIENTED_EDGE('',*,*,#6564,.F.);
#8687=ORIENTED_EDGE('',*,*,#6542,.T.);
#8688=ORIENTED_EDGE('',*,*,#6539,.T.);
#8689=ORIENTED_EDGE('',*,*,#6536,.T.);
#8690=ORIENTED_EDGE('',*,*,#6533,.T.);
#8691=ORIENTED_EDGE('',*,*,#6530,.T.);
#8692=ORIENTED_EDGE('',*,*,#6527,.T.);
#8693=ORIENTED_EDGE('',*,*,#6524,.T.);
#8694=ORIENTED_EDGE('',*,*,#6521,.T.);
#8695=ORIENTED_EDGE('',*,*,#6517,.T.);
#8696=ORIENTED_EDGE('',*,*,#6567,.F.);
#8697=ORIENTED_EDGE('',*,*,#6548,.F.);
#8698=ORIENTED_EDGE('',*,*,#6458,.T.);
#8699=ORIENTED_EDGE('',*,*,#6455,.T.);
#8700=ORIENTED_EDGE('',*,*,#6452,.T.);
#8701=ORIENTED_EDGE('',*,*,#6449,.T.);
#8702=ORIENTED_EDGE('',*,*,#6446,.T.);
#8703=ORIENTED_EDGE('',*,*,#6443,.T.);
#8704=ORIENTED_EDGE('',*,*,#6440,.T.);
#8705=ORIENTED_EDGE('',*,*,#6437,.T.);
#8706=ORIENTED_EDGE('',*,*,#6545,.T.);
#8707=ORIENTED_EDGE('',*,*,#6568,.F.);
#8708=ORIENTED_EDGE('',*,*,#6569,.F.);
#8709=ORIENTED_EDGE('',*,*,#6570,.F.);
#8710=ORIENTED_EDGE('',*,*,#6571,.F.);
#8711=ORIENTED_EDGE('',*,*,#6570,.T.);
#8712=ORIENTED_EDGE('',*,*,#6572,.T.);
#8713=ORIENTED_EDGE('',*,*,#6573,.F.);
#8714=ORIENTED_EDGE('',*,*,#6574,.F.);
#8715=ORIENTED_EDGE('',*,*,#6575,.T.);
#8716=ORIENTED_EDGE('',*,*,#6576,.T.);
#8717=ORIENTED_EDGE('',*,*,#6577,.T.);
#8718=ORIENTED_EDGE('',*,*,#6573,.T.);
#8719=ORIENTED_EDGE('',*,*,#6578,.T.);
#8720=ORIENTED_EDGE('',*,*,#6575,.F.);
#8721=ORIENTED_EDGE('',*,*,#6572,.F.);
#8722=ORIENTED_EDGE('',*,*,#6569,.T.);
#8723=ORIENTED_EDGE('',*,*,#6579,.F.);
#8724=ORIENTED_EDGE('',*,*,#6580,.F.);
#8725=ORIENTED_EDGE('',*,*,#6581,.T.);
#8726=ORIENTED_EDGE('',*,*,#6582,.F.);
#8727=ORIENTED_EDGE('',*,*,#6583,.T.);
#8728=ORIENTED_EDGE('',*,*,#6584,.T.);
#8729=ORIENTED_EDGE('',*,*,#6585,.T.);
#8730=ORIENTED_EDGE('',*,*,#6586,.T.);
#8731=ORIENTED_EDGE('',*,*,#6587,.T.);
#8732=ORIENTED_EDGE('',*,*,#6576,.F.);
#8733=ORIENTED_EDGE('',*,*,#6585,.F.);
#8734=ORIENTED_EDGE('',*,*,#6588,.F.);
#8735=ORIENTED_EDGE('',*,*,#6589,.F.);
#8736=ORIENTED_EDGE('',*,*,#6586,.F.);
#8737=ORIENTED_EDGE('',*,*,#6584,.F.);
#8738=ORIENTED_EDGE('',*,*,#6577,.F.);
#8739=ORIENTED_EDGE('',*,*,#6587,.F.);
#8740=ORIENTED_EDGE('',*,*,#6589,.T.);
#8741=ORIENTED_EDGE('',*,*,#6590,.F.);
#8742=ORIENTED_EDGE('',*,*,#6591,.F.);
#8743=ORIENTED_EDGE('',*,*,#6592,.T.);
#8744=ORIENTED_EDGE('',*,*,#6593,.F.);
#8745=ORIENTED_EDGE('',*,*,#6594,.T.);
#8746=ORIENTED_EDGE('',*,*,#6571,.T.);
#8747=ORIENTED_EDGE('',*,*,#6574,.T.);
#8748=ORIENTED_EDGE('',*,*,#6588,.T.);
#8749=ORIENTED_EDGE('',*,*,#6583,.F.);
#8750=ORIENTED_EDGE('',*,*,#6595,.F.);
#8751=ORIENTED_EDGE('',*,*,#6590,.T.);
#8752=ORIENTED_EDGE('',*,*,#6591,.T.);
#8753=ORIENTED_EDGE('',*,*,#6595,.T.);
#8754=ORIENTED_EDGE('',*,*,#6582,.T.);
#8755=ORIENTED_EDGE('',*,*,#6596,.T.);
#8756=ORIENTED_EDGE('',*,*,#6597,.T.);
#8757=ORIENTED_EDGE('',*,*,#6598,.T.);
#8758=ORIENTED_EDGE('',*,*,#6597,.F.);
#8759=ORIENTED_EDGE('',*,*,#6599,.F.);
#8760=ORIENTED_EDGE('',*,*,#6600,.T.);
#8761=ORIENTED_EDGE('',*,*,#6578,.F.);
#8762=ORIENTED_EDGE('',*,*,#6600,.F.);
#8763=ORIENTED_EDGE('',*,*,#6601,.F.);
#8764=ORIENTED_EDGE('',*,*,#6602,.F.);
#8765=ORIENTED_EDGE('',*,*,#6603,.F.);
#8766=ORIENTED_EDGE('',*,*,#6596,.F.);
#8767=ORIENTED_EDGE('',*,*,#6581,.F.);
#8768=ORIENTED_EDGE('',*,*,#6604,.F.);
#8769=ORIENTED_EDGE('',*,*,#6601,.T.);
#8770=ORIENTED_EDGE('',*,*,#6599,.T.);
#8771=ORIENTED_EDGE('',*,*,#6598,.F.);
#8772=ORIENTED_EDGE('',*,*,#6603,.T.);
#8773=ORIENTED_EDGE('',*,*,#6605,.F.);
#8774=ORIENTED_EDGE('',*,*,#6592,.F.);
#8775=ORIENTED_EDGE('',*,*,#6580,.T.);
#8776=ORIENTED_EDGE('',*,*,#6606,.T.);
#8777=ORIENTED_EDGE('',*,*,#6593,.T.);
#8778=ORIENTED_EDGE('',*,*,#6605,.T.);
#8779=ORIENTED_EDGE('',*,*,#6602,.T.);
#8780=ORIENTED_EDGE('',*,*,#6604,.T.);
#8781=ORIENTED_EDGE('',*,*,#6568,.T.);
#8782=ORIENTED_EDGE('',*,*,#6594,.F.);
#8783=ORIENTED_EDGE('',*,*,#6606,.F.);
#8784=ORIENTED_EDGE('',*,*,#6579,.T.);
#8785=ORIENTED_EDGE('',*,*,#6607,.T.);
#8786=ORIENTED_EDGE('',*,*,#6608,.T.);
#8787=ORIENTED_EDGE('',*,*,#6609,.T.);
#8788=ORIENTED_EDGE('',*,*,#6610,.F.);
#8789=ORIENTED_EDGE('',*,*,#6611,.T.);
#8790=ORIENTED_EDGE('',*,*,#6612,.T.);
#8791=ORIENTED_EDGE('',*,*,#6613,.T.);
#8792=ORIENTED_EDGE('',*,*,#6608,.F.);
#8793=ORIENTED_EDGE('',*,*,#6614,.T.);
#8794=ORIENTED_EDGE('',*,*,#6615,.T.);
#8795=ORIENTED_EDGE('',*,*,#6616,.T.);
#8796=ORIENTED_EDGE('',*,*,#6612,.F.);
#8797=ORIENTED_EDGE('',*,*,#6617,.T.);
#8798=ORIENTED_EDGE('',*,*,#6618,.T.);
#8799=ORIENTED_EDGE('',*,*,#6619,.T.);
#8800=ORIENTED_EDGE('',*,*,#6615,.F.);
#8801=ORIENTED_EDGE('',*,*,#6620,.T.);
#8802=ORIENTED_EDGE('',*,*,#6621,.T.);
#8803=ORIENTED_EDGE('',*,*,#6622,.T.);
#8804=ORIENTED_EDGE('',*,*,#6618,.F.);
#8805=ORIENTED_EDGE('',*,*,#6623,.T.);
#8806=ORIENTED_EDGE('',*,*,#6610,.T.);
#8807=ORIENTED_EDGE('',*,*,#6624,.T.);
#8808=ORIENTED_EDGE('',*,*,#6621,.F.);
#8809=ORIENTED_EDGE('',*,*,#6623,.F.);
#8810=ORIENTED_EDGE('',*,*,#6620,.F.);
#8811=ORIENTED_EDGE('',*,*,#6617,.F.);
#8812=ORIENTED_EDGE('',*,*,#6614,.F.);
#8813=ORIENTED_EDGE('',*,*,#6611,.F.);
#8814=ORIENTED_EDGE('',*,*,#6607,.F.);
#8815=ORIENTED_EDGE('',*,*,#6624,.F.);
#8816=ORIENTED_EDGE('',*,*,#6609,.F.);
#8817=ORIENTED_EDGE('',*,*,#6613,.F.);
#8818=ORIENTED_EDGE('',*,*,#6616,.F.);
#8819=ORIENTED_EDGE('',*,*,#6619,.F.);
#8820=ORIENTED_EDGE('',*,*,#6622,.F.);
#8821=ORIENTED_EDGE('',*,*,#6625,.F.);
#8822=ORIENTED_EDGE('',*,*,#6626,.F.);
#8823=ORIENTED_EDGE('',*,*,#6627,.F.);
#8824=ORIENTED_EDGE('',*,*,#6628,.T.);
#8825=ORIENTED_EDGE('',*,*,#6626,.T.);
#8826=ORIENTED_EDGE('',*,*,#6628,.F.);
#8827=ORIENTED_EDGE('',*,*,#6629,.F.);
#8828=ORIENTED_EDGE('',*,*,#6630,.T.);
#8829=ORIENTED_EDGE('',*,*,#6627,.T.);
#8830=ORIENTED_EDGE('',*,*,#6630,.F.);
#8831=ORIENTED_EDGE('',*,*,#6631,.F.);
#8832=ORIENTED_EDGE('',*,*,#6632,.T.);
#8833=ORIENTED_EDGE('',*,*,#6629,.T.);
#8834=ORIENTED_EDGE('',*,*,#6632,.F.);
#8835=ORIENTED_EDGE('',*,*,#6631,.T.);
#8836=ORIENTED_EDGE('',*,*,#6633,.F.);
#8837=ORIENTED_EDGE('',*,*,#6634,.F.);
#8838=ORIENTED_EDGE('',*,*,#6635,.T.);
#8839=ORIENTED_EDGE('',*,*,#6633,.T.);
#8840=ORIENTED_EDGE('',*,*,#6635,.F.);
#8841=ORIENTED_EDGE('',*,*,#6625,.T.);
#8842=ORIENTED_EDGE('',*,*,#6636,.T.);
#8843=ORIENTED_EDGE('',*,*,#6634,.T.);
#8844=ORIENTED_EDGE('',*,*,#6636,.F.);
#8845=ORIENTED_EDGE('',*,*,#6637,.F.);
#8846=ORIENTED_EDGE('',*,*,#6638,.T.);
#8847=ORIENTED_EDGE('',*,*,#6639,.F.);
#8848=ORIENTED_EDGE('',*,*,#6638,.F.);
#8849=ORIENTED_EDGE('',*,*,#6637,.T.);
#8850=ORIENTED_EDGE('',*,*,#6640,.F.);
#8851=ORIENTED_EDGE('',*,*,#6641,.F.);
#8852=ORIENTED_EDGE('',*,*,#6642,.T.);
#8853=ORIENTED_EDGE('',*,*,#6643,.F.);
#8854=ORIENTED_EDGE('',*,*,#6642,.F.);
#8855=ORIENTED_EDGE('',*,*,#6641,.T.);
#8856=ORIENTED_EDGE('',*,*,#6644,.F.);
#8857=ORIENTED_EDGE('',*,*,#6645,.F.);
#8858=ORIENTED_EDGE('',*,*,#6646,.T.);
#8859=ORIENTED_EDGE('',*,*,#6647,.F.);
#8860=ORIENTED_EDGE('',*,*,#6646,.F.);
#8861=ORIENTED_EDGE('',*,*,#6645,.T.);
#8862=ORIENTED_EDGE('',*,*,#6648,.F.);
#8863=ORIENTED_EDGE('',*,*,#6649,.F.);
#8864=ORIENTED_EDGE('',*,*,#6650,.T.);
#8865=ORIENTED_EDGE('',*,*,#6651,.F.);
#8866=ORIENTED_EDGE('',*,*,#6650,.F.);
#8867=ORIENTED_EDGE('',*,*,#6649,.T.);
#8868=ORIENTED_EDGE('',*,*,#6652,.F.);
#8869=ORIENTED_EDGE('',*,*,#6653,.F.);
#8870=ORIENTED_EDGE('',*,*,#6654,.T.);
#8871=ORIENTED_EDGE('',*,*,#6640,.T.);
#8872=ORIENTED_EDGE('',*,*,#6654,.F.);
#8873=ORIENTED_EDGE('',*,*,#6655,.F.);
#8874=ORIENTED_EDGE('',*,*,#6656,.T.);
#8875=ORIENTED_EDGE('',*,*,#6644,.T.);
#8876=ORIENTED_EDGE('',*,*,#6656,.F.);
#8877=ORIENTED_EDGE('',*,*,#6657,.F.);
#8878=ORIENTED_EDGE('',*,*,#6658,.T.);
#8879=ORIENTED_EDGE('',*,*,#6648,.T.);
#8880=ORIENTED_EDGE('',*,*,#6658,.F.);
#8881=ORIENTED_EDGE('',*,*,#6659,.F.);
#8882=ORIENTED_EDGE('',*,*,#6660,.T.);
#8883=ORIENTED_EDGE('',*,*,#6652,.T.);
#8884=ORIENTED_EDGE('',*,*,#6660,.F.);
#8885=ORIENTED_EDGE('',*,*,#6661,.T.);
#8886=ORIENTED_EDGE('',*,*,#6662,.T.);
#8887=ORIENTED_EDGE('',*,*,#6663,.F.);
#8888=ORIENTED_EDGE('',*,*,#6664,.F.);
#8889=ORIENTED_EDGE('',*,*,#6665,.T.);
#8890=ORIENTED_EDGE('',*,*,#6664,.T.);
#8891=ORIENTED_EDGE('',*,*,#6666,.F.);
#8892=ORIENTED_EDGE('',*,*,#6667,.F.);
#8893=ORIENTED_EDGE('',*,*,#6668,.T.);
#8894=ORIENTED_EDGE('',*,*,#6667,.T.);
#8895=ORIENTED_EDGE('',*,*,#6669,.F.);
#8896=ORIENTED_EDGE('',*,*,#6670,.F.);
#8897=ORIENTED_EDGE('',*,*,#6671,.T.);
#8898=ORIENTED_EDGE('',*,*,#6670,.T.);
#8899=ORIENTED_EDGE('',*,*,#6672,.F.);
#8900=ORIENTED_EDGE('',*,*,#6673,.F.);
#8901=ORIENTED_EDGE('',*,*,#6674,.T.);
#8902=ORIENTED_EDGE('',*,*,#6673,.T.);
#8903=ORIENTED_EDGE('',*,*,#6675,.F.);
#8904=ORIENTED_EDGE('',*,*,#6676,.F.);
#8905=ORIENTED_EDGE('',*,*,#6651,.T.);
#8906=ORIENTED_EDGE('',*,*,#6647,.T.);
#8907=ORIENTED_EDGE('',*,*,#6643,.T.);
#8908=ORIENTED_EDGE('',*,*,#6639,.T.);
#8909=ORIENTED_EDGE('',*,*,#6677,.T.);
#8910=ORIENTED_EDGE('',*,*,#6676,.T.);
#8911=ORIENTED_EDGE('',*,*,#6678,.F.);
#8912=ORIENTED_EDGE('',*,*,#6679,.F.);
#8913=ORIENTED_EDGE('',*,*,#6680,.T.);
#8914=ORIENTED_EDGE('',*,*,#6679,.T.);
#8915=ORIENTED_EDGE('',*,*,#6681,.F.);
#8916=ORIENTED_EDGE('',*,*,#6682,.F.);
#8917=ORIENTED_EDGE('',*,*,#6683,.T.);
#8918=ORIENTED_EDGE('',*,*,#6682,.T.);
#8919=ORIENTED_EDGE('',*,*,#6684,.F.);
#8920=ORIENTED_EDGE('',*,*,#6685,.F.);
#8921=ORIENTED_EDGE('',*,*,#6686,.T.);
#8922=ORIENTED_EDGE('',*,*,#6685,.T.);
#8923=ORIENTED_EDGE('',*,*,#6687,.F.);
#8924=ORIENTED_EDGE('',*,*,#6688,.F.);
#8925=ORIENTED_EDGE('',*,*,#6689,.T.);
#8926=ORIENTED_EDGE('',*,*,#6688,.T.);
#8927=ORIENTED_EDGE('',*,*,#6690,.F.);
#8928=ORIENTED_EDGE('',*,*,#6691,.F.);
#8929=ORIENTED_EDGE('',*,*,#6692,.T.);
#8930=ORIENTED_EDGE('',*,*,#6691,.T.);
#8931=ORIENTED_EDGE('',*,*,#6693,.F.);
#8932=ORIENTED_EDGE('',*,*,#6694,.F.);
#8933=ORIENTED_EDGE('',*,*,#6653,.T.);
#8934=ORIENTED_EDGE('',*,*,#6655,.T.);
#8935=ORIENTED_EDGE('',*,*,#6657,.T.);
#8936=ORIENTED_EDGE('',*,*,#6659,.T.);
#8937=ORIENTED_EDGE('',*,*,#6695,.T.);
#8938=ORIENTED_EDGE('',*,*,#6694,.T.);
#8939=ORIENTED_EDGE('',*,*,#6696,.F.);
#8940=ORIENTED_EDGE('',*,*,#6662,.F.);
#8941=ORIENTED_EDGE('',*,*,#6696,.T.);
#8942=ORIENTED_EDGE('',*,*,#6693,.T.);
#8943=ORIENTED_EDGE('',*,*,#6690,.T.);
#8944=ORIENTED_EDGE('',*,*,#6687,.T.);
#8945=ORIENTED_EDGE('',*,*,#6684,.T.);
#8946=ORIENTED_EDGE('',*,*,#6681,.T.);
#8947=ORIENTED_EDGE('',*,*,#6678,.T.);
#8948=ORIENTED_EDGE('',*,*,#6675,.T.);
#8949=ORIENTED_EDGE('',*,*,#6672,.T.);
#8950=ORIENTED_EDGE('',*,*,#6669,.T.);
#8951=ORIENTED_EDGE('',*,*,#6666,.T.);
#8952=ORIENTED_EDGE('',*,*,#6663,.T.);
#8953=ORIENTED_EDGE('',*,*,#6695,.F.);
#8954=ORIENTED_EDGE('',*,*,#6661,.F.);
#8955=ORIENTED_EDGE('',*,*,#6665,.F.);
#8956=ORIENTED_EDGE('',*,*,#6668,.F.);
#8957=ORIENTED_EDGE('',*,*,#6671,.F.);
#8958=ORIENTED_EDGE('',*,*,#6674,.F.);
#8959=ORIENTED_EDGE('',*,*,#6677,.F.);
#8960=ORIENTED_EDGE('',*,*,#6680,.F.);
#8961=ORIENTED_EDGE('',*,*,#6683,.F.);
#8962=ORIENTED_EDGE('',*,*,#6686,.F.);
#8963=ORIENTED_EDGE('',*,*,#6689,.F.);
#8964=ORIENTED_EDGE('',*,*,#6692,.F.);
#8965=ORIENTED_EDGE('',*,*,#6697,.F.);
#8966=ORIENTED_EDGE('',*,*,#6698,.T.);
#8967=ORIENTED_EDGE('',*,*,#6699,.T.);
#8968=ORIENTED_EDGE('',*,*,#6698,.F.);
#8969=ORIENTED_EDGE('',*,*,#6699,.F.);
#8970=ORIENTED_EDGE('',*,*,#6700,.T.);
#8971=ORIENTED_EDGE('',*,*,#6701,.F.);
#8972=ORIENTED_EDGE('',*,*,#6702,.F.);
#8973=ORIENTED_EDGE('',*,*,#6703,.F.);
#8974=ORIENTED_EDGE('',*,*,#6700,.F.);
#8975=ORIENTED_EDGE('',*,*,#6704,.T.);
#8976=ORIENTED_EDGE('',*,*,#6702,.T.);
#8977=ORIENTED_EDGE('',*,*,#6704,.F.);
#8978=ORIENTED_EDGE('',*,*,#6703,.T.);
#8979=ORIENTED_EDGE('',*,*,#6705,.T.);
#8980=ORIENTED_EDGE('',*,*,#6706,.T.);
#8981=ORIENTED_EDGE('',*,*,#6705,.F.);
#8982=ORIENTED_EDGE('',*,*,#6707,.F.);
#8983=ORIENTED_EDGE('',*,*,#6708,.T.);
#8984=ORIENTED_EDGE('',*,*,#6709,.T.);
#8985=ORIENTED_EDGE('',*,*,#6708,.F.);
#8986=ORIENTED_EDGE('',*,*,#6709,.F.);
#8987=ORIENTED_EDGE('',*,*,#6697,.T.);
#8988=ORIENTED_EDGE('',*,*,#6710,.F.);
#8989=ORIENTED_EDGE('',*,*,#6711,.T.);
#8990=ORIENTED_EDGE('',*,*,#6701,.T.);
#8991=ORIENTED_EDGE('',*,*,#6711,.F.);
#8992=ORIENTED_EDGE('',*,*,#6710,.T.);
#8993=ORIENTED_EDGE('',*,*,#6706,.F.);
#8994=ORIENTED_EDGE('',*,*,#6707,.T.);
#8995=ORIENTED_EDGE('',*,*,#6712,.F.);
#8996=ORIENTED_EDGE('',*,*,#6713,.T.);
#8997=ORIENTED_EDGE('',*,*,#6714,.F.);
#8998=ORIENTED_EDGE('',*,*,#6713,.F.);
#8999=ORIENTED_EDGE('',*,*,#6712,.T.);
#9000=ORIENTED_EDGE('',*,*,#6715,.F.);
#9001=ORIENTED_EDGE('',*,*,#6715,.T.);
#9002=ORIENTED_EDGE('',*,*,#6716,.T.);
#9003=ORIENTED_EDGE('',*,*,#6717,.T.);
#9004=ORIENTED_EDGE('',*,*,#6716,.F.);
#9005=ORIENTED_EDGE('',*,*,#6718,.F.);
#9006=ORIENTED_EDGE('',*,*,#6719,.T.);
#9007=ORIENTED_EDGE('',*,*,#6720,.T.);
#9008=ORIENTED_EDGE('',*,*,#6719,.F.);
#9009=ORIENTED_EDGE('',*,*,#6718,.T.);
#9010=ORIENTED_EDGE('',*,*,#6714,.T.);
#9011=ORIENTED_EDGE('',*,*,#6720,.F.);
#9012=ORIENTED_EDGE('',*,*,#6717,.F.);
#9013=ORIENTED_EDGE('',*,*,#6721,.F.);
#9014=ORIENTED_EDGE('',*,*,#6722,.T.);
#9015=ORIENTED_EDGE('',*,*,#6723,.T.);
#9016=ORIENTED_EDGE('',*,*,#6722,.F.);
#9017=ORIENTED_EDGE('',*,*,#6724,.F.);
#9018=ORIENTED_EDGE('',*,*,#6725,.T.);
#9019=ORIENTED_EDGE('',*,*,#6726,.T.);
#9020=ORIENTED_EDGE('',*,*,#6725,.F.);
#9021=ORIENTED_EDGE('',*,*,#6724,.T.);
#9022=ORIENTED_EDGE('',*,*,#6721,.T.);
#9023=ORIENTED_EDGE('',*,*,#6726,.F.);
#9024=ORIENTED_EDGE('',*,*,#6723,.F.);
#9025=ORIENTED_EDGE('',*,*,#6727,.F.);
#9026=ORIENTED_EDGE('',*,*,#6728,.T.);
#9027=ORIENTED_EDGE('',*,*,#6729,.T.);
#9028=ORIENTED_EDGE('',*,*,#6728,.F.);
#9029=ORIENTED_EDGE('',*,*,#6727,.T.);
#9030=ORIENTED_EDGE('',*,*,#6729,.F.);
#9031=ORIENTED_EDGE('',*,*,#6730,.F.);
#9032=ORIENTED_EDGE('',*,*,#6731,.T.);
#9033=ORIENTED_EDGE('',*,*,#6732,.T.);
#9034=ORIENTED_EDGE('',*,*,#6731,.F.);
#9035=ORIENTED_EDGE('',*,*,#6730,.T.);
#9036=ORIENTED_EDGE('',*,*,#6732,.F.);
#9037=ORIENTED_EDGE('',*,*,#6733,.F.);
#9038=ORIENTED_EDGE('',*,*,#6734,.T.);
#9039=ORIENTED_EDGE('',*,*,#6735,.T.);
#9040=ORIENTED_EDGE('',*,*,#6734,.F.);
#9041=ORIENTED_EDGE('',*,*,#6736,.F.);
#9042=ORIENTED_EDGE('',*,*,#6737,.T.);
#9043=ORIENTED_EDGE('',*,*,#6738,.T.);
#9044=ORIENTED_EDGE('',*,*,#6737,.F.);
#9045=ORIENTED_EDGE('',*,*,#6736,.T.);
#9046=ORIENTED_EDGE('',*,*,#6733,.T.);
#9047=ORIENTED_EDGE('',*,*,#6738,.F.);
#9048=ORIENTED_EDGE('',*,*,#6735,.F.);
#9049=ORIENTED_EDGE('',*,*,#6739,.F.);
#9050=ORIENTED_EDGE('',*,*,#6740,.T.);
#9051=ORIENTED_EDGE('',*,*,#6741,.T.);
#9052=ORIENTED_EDGE('',*,*,#6740,.F.);
#9053=ORIENTED_EDGE('',*,*,#6741,.F.);
#9054=ORIENTED_EDGE('',*,*,#6742,.T.);
#9055=ORIENTED_EDGE('',*,*,#6743,.F.);
#9056=ORIENTED_EDGE('',*,*,#6744,.F.);
#9057=ORIENTED_EDGE('',*,*,#6745,.F.);
#9058=ORIENTED_EDGE('',*,*,#6742,.F.);
#9059=ORIENTED_EDGE('',*,*,#6746,.T.);
#9060=ORIENTED_EDGE('',*,*,#6744,.T.);
#9061=ORIENTED_EDGE('',*,*,#6746,.F.);
#9062=ORIENTED_EDGE('',*,*,#6745,.T.);
#9063=ORIENTED_EDGE('',*,*,#6747,.T.);
#9064=ORIENTED_EDGE('',*,*,#6748,.T.);
#9065=ORIENTED_EDGE('',*,*,#6747,.F.);
#9066=ORIENTED_EDGE('',*,*,#6749,.F.);
#9067=ORIENTED_EDGE('',*,*,#6750,.T.);
#9068=ORIENTED_EDGE('',*,*,#6751,.T.);
#9069=ORIENTED_EDGE('',*,*,#6750,.F.);
#9070=ORIENTED_EDGE('',*,*,#6751,.F.);
#9071=ORIENTED_EDGE('',*,*,#6739,.T.);
#9072=ORIENTED_EDGE('',*,*,#6752,.F.);
#9073=ORIENTED_EDGE('',*,*,#6753,.T.);
#9074=ORIENTED_EDGE('',*,*,#6743,.T.);
#9075=ORIENTED_EDGE('',*,*,#6753,.F.);
#9076=ORIENTED_EDGE('',*,*,#6752,.T.);
#9077=ORIENTED_EDGE('',*,*,#6748,.F.);
#9078=ORIENTED_EDGE('',*,*,#6749,.T.);
#9079=ORIENTED_EDGE('',*,*,#6754,.F.);
#9080=ORIENTED_EDGE('',*,*,#6755,.T.);
#9081=ORIENTED_EDGE('',*,*,#6756,.F.);
#9082=ORIENTED_EDGE('',*,*,#6755,.F.);
#9083=ORIENTED_EDGE('',*,*,#6754,.T.);
#9084=ORIENTED_EDGE('',*,*,#6757,.F.);
#9085=ORIENTED_EDGE('',*,*,#6757,.T.);
#9086=ORIENTED_EDGE('',*,*,#6758,.T.);
#9087=ORIENTED_EDGE('',*,*,#6759,.T.);
#9088=ORIENTED_EDGE('',*,*,#6758,.F.);
#9089=ORIENTED_EDGE('',*,*,#6760,.F.);
#9090=ORIENTED_EDGE('',*,*,#6761,.T.);
#9091=ORIENTED_EDGE('',*,*,#6762,.T.);
#9092=ORIENTED_EDGE('',*,*,#6761,.F.);
#9093=ORIENTED_EDGE('',*,*,#6760,.T.);
#9094=ORIENTED_EDGE('',*,*,#6756,.T.);
#9095=ORIENTED_EDGE('',*,*,#6762,.F.);
#9096=ORIENTED_EDGE('',*,*,#6759,.F.);
#9097=ORIENTED_EDGE('',*,*,#6763,.F.);
#9098=ORIENTED_EDGE('',*,*,#6764,.T.);
#9099=ORIENTED_EDGE('',*,*,#6765,.T.);
#9100=ORIENTED_EDGE('',*,*,#6764,.F.);
#9101=ORIENTED_EDGE('',*,*,#6766,.F.);
#9102=ORIENTED_EDGE('',*,*,#6767,.T.);
#9103=ORIENTED_EDGE('',*,*,#6768,.T.);
#9104=ORIENTED_EDGE('',*,*,#6767,.F.);
#9105=ORIENTED_EDGE('',*,*,#6766,.T.);
#9106=ORIENTED_EDGE('',*,*,#6763,.T.);
#9107=ORIENTED_EDGE('',*,*,#6768,.F.);
#9108=ORIENTED_EDGE('',*,*,#6765,.F.);
#9109=ORIENTED_EDGE('',*,*,#6769,.F.);
#9110=ORIENTED_EDGE('',*,*,#6770,.T.);
#9111=ORIENTED_EDGE('',*,*,#6771,.T.);
#9112=ORIENTED_EDGE('',*,*,#6770,.F.);
#9113=ORIENTED_EDGE('',*,*,#6769,.T.);
#9114=ORIENTED_EDGE('',*,*,#6771,.F.);
#9115=ORIENTED_EDGE('',*,*,#6772,.F.);
#9116=ORIENTED_EDGE('',*,*,#6773,.T.);
#9117=ORIENTED_EDGE('',*,*,#6774,.T.);
#9118=ORIENTED_EDGE('',*,*,#6773,.F.);
#9119=ORIENTED_EDGE('',*,*,#6772,.T.);
#9120=ORIENTED_EDGE('',*,*,#6774,.F.);
#9121=ORIENTED_EDGE('',*,*,#6775,.F.);
#9122=ORIENTED_EDGE('',*,*,#6776,.T.);
#9123=ORIENTED_EDGE('',*,*,#6777,.T.);
#9124=ORIENTED_EDGE('',*,*,#6776,.F.);
#9125=ORIENTED_EDGE('',*,*,#6778,.F.);
#9126=ORIENTED_EDGE('',*,*,#6779,.T.);
#9127=ORIENTED_EDGE('',*,*,#6780,.T.);
#9128=ORIENTED_EDGE('',*,*,#6779,.F.);
#9129=ORIENTED_EDGE('',*,*,#6778,.T.);
#9130=ORIENTED_EDGE('',*,*,#6775,.T.);
#9131=ORIENTED_EDGE('',*,*,#6780,.F.);
#9132=ORIENTED_EDGE('',*,*,#6777,.F.);
#9133=ORIENTED_EDGE('',*,*,#6781,.F.);
#9134=ORIENTED_EDGE('',*,*,#6782,.F.);
#9135=ORIENTED_EDGE('',*,*,#6783,.F.);
#9136=ORIENTED_EDGE('',*,*,#6784,.T.);
#9137=ORIENTED_EDGE('',*,*,#6785,.F.);
#9138=ORIENTED_EDGE('',*,*,#6786,.F.);
#9139=ORIENTED_EDGE('',*,*,#6787,.F.);
#9140=ORIENTED_EDGE('',*,*,#6788,.F.);
#9141=ORIENTED_EDGE('',*,*,#6784,.F.);
#9142=ORIENTED_EDGE('',*,*,#6789,.F.);
#9143=ORIENTED_EDGE('',*,*,#6790,.F.);
#9144=ORIENTED_EDGE('',*,*,#6791,.T.);
#9145=ORIENTED_EDGE('',*,*,#6792,.F.);
#9146=ORIENTED_EDGE('',*,*,#6793,.F.);
#9147=ORIENTED_EDGE('',*,*,#6794,.F.);
#9148=ORIENTED_EDGE('',*,*,#6791,.F.);
#9149=ORIENTED_EDGE('',*,*,#6795,.F.);
#9150=ORIENTED_EDGE('',*,*,#6796,.T.);
#9151=ORIENTED_EDGE('',*,*,#6782,.T.);
#9152=ORIENTED_EDGE('',*,*,#6797,.T.);
#9153=ORIENTED_EDGE('',*,*,#6798,.F.);
#9154=ORIENTED_EDGE('',*,*,#6797,.F.);
#9155=ORIENTED_EDGE('',*,*,#6781,.T.);
#9156=ORIENTED_EDGE('',*,*,#6783,.T.);
#9157=ORIENTED_EDGE('',*,*,#6796,.F.);
#9158=ORIENTED_EDGE('',*,*,#6793,.T.);
#9159=ORIENTED_EDGE('',*,*,#6792,.T.);
#9160=ORIENTED_EDGE('',*,*,#6794,.T.);
#9161=ORIENTED_EDGE('',*,*,#6799,.T.);
#9162=ORIENTED_EDGE('',*,*,#6800,.T.);
#9163=ORIENTED_EDGE('',*,*,#6801,.T.);
#9164=ORIENTED_EDGE('',*,*,#6802,.T.);
#9165=ORIENTED_EDGE('',*,*,#6803,.T.);
#9166=ORIENTED_EDGE('',*,*,#6804,.T.);
#9167=ORIENTED_EDGE('',*,*,#6800,.F.);
#9168=ORIENTED_EDGE('',*,*,#6799,.F.);
#9169=ORIENTED_EDGE('',*,*,#6801,.F.);
#9170=ORIENTED_EDGE('',*,*,#6805,.T.);
#9171=ORIENTED_EDGE('',*,*,#6806,.F.);
#9172=ORIENTED_EDGE('',*,*,#6807,.F.);
#9173=ORIENTED_EDGE('',*,*,#6805,.F.);
#9174=ORIENTED_EDGE('',*,*,#6808,.F.);
#9175=ORIENTED_EDGE('',*,*,#6809,.F.);
#9176=ORIENTED_EDGE('',*,*,#6810,.T.);
#9177=ORIENTED_EDGE('',*,*,#6803,.F.);
#9178=ORIENTED_EDGE('',*,*,#6802,.F.);
#9179=ORIENTED_EDGE('',*,*,#6804,.F.);
#9180=ORIENTED_EDGE('',*,*,#6810,.F.);
#9181=ORIENTED_EDGE('',*,*,#6811,.F.);
#9182=ORIENTED_EDGE('',*,*,#6812,.T.);
#9183=ORIENTED_EDGE('',*,*,#6785,.T.);
#9184=ORIENTED_EDGE('',*,*,#6788,.T.);
#9185=ORIENTED_EDGE('',*,*,#6813,.T.);
#9186=ORIENTED_EDGE('',*,*,#6814,.F.);
#9187=ORIENTED_EDGE('',*,*,#6813,.F.);
#9188=ORIENTED_EDGE('',*,*,#6787,.T.);
#9189=ORIENTED_EDGE('',*,*,#6786,.T.);
#9190=ORIENTED_EDGE('',*,*,#6812,.F.);
#9191=ORIENTED_EDGE('',*,*,#6789,.T.);
#9192=ORIENTED_EDGE('',*,*,#6790,.T.);
#9193=ORIENTED_EDGE('',*,*,#6808,.T.);
#9194=ORIENTED_EDGE('',*,*,#6809,.T.);
#9195=ORIENTED_EDGE('',*,*,#6806,.T.);
#9196=ORIENTED_EDGE('',*,*,#6807,.T.);
#9197=ORIENTED_EDGE('',*,*,#6795,.T.);
#9198=ORIENTED_EDGE('',*,*,#6811,.T.);
#9199=ORIENTED_EDGE('',*,*,#6815,.T.);
#9200=ORIENTED_EDGE('',*,*,#6816,.T.);
#9201=ORIENTED_EDGE('',*,*,#6817,.F.);
#9202=ORIENTED_EDGE('',*,*,#6818,.T.);
#9203=ORIENTED_EDGE('',*,*,#6819,.F.);
#9204=ORIENTED_EDGE('',*,*,#6820,.T.);
#9205=ORIENTED_EDGE('',*,*,#6821,.F.);
#9206=ORIENTED_EDGE('',*,*,#6822,.T.);
#9207=ORIENTED_EDGE('',*,*,#6823,.F.);
#9208=ORIENTED_EDGE('',*,*,#6824,.T.);
#9209=ORIENTED_EDGE('',*,*,#6825,.F.);
#9210=ORIENTED_EDGE('',*,*,#6826,.T.);
#9211=ORIENTED_EDGE('',*,*,#6827,.F.);
#9212=ORIENTED_EDGE('',*,*,#6828,.T.);
#9213=ORIENTED_EDGE('',*,*,#6829,.F.);
#9214=ORIENTED_EDGE('',*,*,#6830,.T.);
#9215=ORIENTED_EDGE('',*,*,#6831,.F.);
#9216=ORIENTED_EDGE('',*,*,#6832,.T.);
#9217=ORIENTED_EDGE('',*,*,#6833,.F.);
#9218=ORIENTED_EDGE('',*,*,#6834,.T.);
#9219=ORIENTED_EDGE('',*,*,#6835,.F.);
#9220=ORIENTED_EDGE('',*,*,#6836,.T.);
#9221=ORIENTED_EDGE('',*,*,#6837,.F.);
#9222=ORIENTED_EDGE('',*,*,#6838,.T.);
#9223=ORIENTED_EDGE('',*,*,#6839,.F.);
#9224=ORIENTED_EDGE('',*,*,#6840,.T.);
#9225=ORIENTED_EDGE('',*,*,#6841,.F.);
#9226=ORIENTED_EDGE('',*,*,#6842,.T.);
#9227=ORIENTED_EDGE('',*,*,#6843,.F.);
#9228=ORIENTED_EDGE('',*,*,#6844,.T.);
#9229=ORIENTED_EDGE('',*,*,#6845,.F.);
#9230=ORIENTED_EDGE('',*,*,#6846,.T.);
#9231=ORIENTED_EDGE('',*,*,#6847,.F.);
#9232=ORIENTED_EDGE('',*,*,#6848,.T.);
#9233=ORIENTED_EDGE('',*,*,#6849,.F.);
#9234=ORIENTED_EDGE('',*,*,#6850,.T.);
#9235=ORIENTED_EDGE('',*,*,#6851,.F.);
#9236=ORIENTED_EDGE('',*,*,#6852,.T.);
#9237=ORIENTED_EDGE('',*,*,#6853,.F.);
#9238=ORIENTED_EDGE('',*,*,#6854,.T.);
#9239=ORIENTED_EDGE('',*,*,#6855,.F.);
#9240=ORIENTED_EDGE('',*,*,#6856,.F.);
#9241=ORIENTED_EDGE('',*,*,#6857,.T.);
#9242=ORIENTED_EDGE('',*,*,#6815,.F.);
#9243=ORIENTED_EDGE('',*,*,#6857,.F.);
#9244=ORIENTED_EDGE('',*,*,#6856,.T.);
#9245=ORIENTED_EDGE('',*,*,#6798,.T.);
#9246=ORIENTED_EDGE('',*,*,#6858,.F.);
#9247=ORIENTED_EDGE('',*,*,#6859,.T.);
#9248=ORIENTED_EDGE('',*,*,#6860,.T.);
#9249=ORIENTED_EDGE('',*,*,#6861,.T.);
#9250=ORIENTED_EDGE('',*,*,#6862,.T.);
#9251=ORIENTED_EDGE('',*,*,#6863,.T.);
#9252=ORIENTED_EDGE('',*,*,#6864,.T.);
#9253=ORIENTED_EDGE('',*,*,#6865,.T.);
#9254=ORIENTED_EDGE('',*,*,#6866,.T.);
#9255=ORIENTED_EDGE('',*,*,#6867,.T.);
#9256=ORIENTED_EDGE('',*,*,#6868,.T.);
#9257=ORIENTED_EDGE('',*,*,#6869,.T.);
#9258=ORIENTED_EDGE('',*,*,#6870,.T.);
#9259=ORIENTED_EDGE('',*,*,#6871,.T.);
#9260=ORIENTED_EDGE('',*,*,#6872,.T.);
#9261=ORIENTED_EDGE('',*,*,#6873,.T.);
#9262=ORIENTED_EDGE('',*,*,#6874,.T.);
#9263=ORIENTED_EDGE('',*,*,#6875,.T.);
#9264=ORIENTED_EDGE('',*,*,#6876,.T.);
#9265=ORIENTED_EDGE('',*,*,#6877,.T.);
#9266=ORIENTED_EDGE('',*,*,#6878,.T.);
#9267=ORIENTED_EDGE('',*,*,#6879,.T.);
#9268=ORIENTED_EDGE('',*,*,#6880,.T.);
#9269=ORIENTED_EDGE('',*,*,#6881,.T.);
#9270=ORIENTED_EDGE('',*,*,#6882,.T.);
#9271=ORIENTED_EDGE('',*,*,#6883,.T.);
#9272=ORIENTED_EDGE('',*,*,#6884,.T.);
#9273=ORIENTED_EDGE('',*,*,#6885,.T.);
#9274=ORIENTED_EDGE('',*,*,#6886,.T.);
#9275=ORIENTED_EDGE('',*,*,#6887,.T.);
#9276=ORIENTED_EDGE('',*,*,#6888,.T.);
#9277=ORIENTED_EDGE('',*,*,#6889,.T.);
#9278=ORIENTED_EDGE('',*,*,#6890,.T.);
#9279=ORIENTED_EDGE('',*,*,#6891,.T.);
#9280=ORIENTED_EDGE('',*,*,#6892,.T.);
#9281=ORIENTED_EDGE('',*,*,#6893,.T.);
#9282=ORIENTED_EDGE('',*,*,#6894,.T.);
#9283=ORIENTED_EDGE('',*,*,#6895,.T.);
#9284=ORIENTED_EDGE('',*,*,#6896,.T.);
#9285=ORIENTED_EDGE('',*,*,#6897,.T.);
#9286=ORIENTED_EDGE('',*,*,#6898,.T.);
#9287=ORIENTED_EDGE('',*,*,#6899,.F.);
#9288=ORIENTED_EDGE('',*,*,#6900,.T.);
#9289=ORIENTED_EDGE('',*,*,#6858,.T.);
#9290=ORIENTED_EDGE('',*,*,#6900,.F.);
#9291=ORIENTED_EDGE('',*,*,#6899,.T.);
#9292=ORIENTED_EDGE('',*,*,#6814,.T.);
#9293=ORIENTED_EDGE('',*,*,#6901,.F.);
#9294=ORIENTED_EDGE('',*,*,#6859,.F.);
#9295=ORIENTED_EDGE('',*,*,#6902,.F.);
#9296=ORIENTED_EDGE('',*,*,#6816,.F.);
#9297=ORIENTED_EDGE('',*,*,#6902,.T.);
#9298=ORIENTED_EDGE('',*,*,#6898,.F.);
#9299=ORIENTED_EDGE('',*,*,#6903,.T.);
#9300=ORIENTED_EDGE('',*,*,#6817,.T.);
#9301=ORIENTED_EDGE('',*,*,#6903,.F.);
#9302=ORIENTED_EDGE('',*,*,#6897,.F.);
#9303=ORIENTED_EDGE('',*,*,#6904,.F.);
#9304=ORIENTED_EDGE('',*,*,#6818,.F.);
#9305=ORIENTED_EDGE('',*,*,#6904,.T.);
#9306=ORIENTED_EDGE('',*,*,#6896,.F.);
#9307=ORIENTED_EDGE('',*,*,#6905,.T.);
#9308=ORIENTED_EDGE('',*,*,#6819,.T.);
#9309=ORIENTED_EDGE('',*,*,#6905,.F.);
#9310=ORIENTED_EDGE('',*,*,#6895,.F.);
#9311=ORIENTED_EDGE('',*,*,#6906,.F.);
#9312=ORIENTED_EDGE('',*,*,#6820,.F.);
#9313=ORIENTED_EDGE('',*,*,#6906,.T.);
#9314=ORIENTED_EDGE('',*,*,#6894,.F.);
#9315=ORIENTED_EDGE('',*,*,#6907,.T.);
#9316=ORIENTED_EDGE('',*,*,#6821,.T.);
#9317=ORIENTED_EDGE('',*,*,#6907,.F.);
#9318=ORIENTED_EDGE('',*,*,#6893,.F.);
#9319=ORIENTED_EDGE('',*,*,#6908,.F.);
#9320=ORIENTED_EDGE('',*,*,#6822,.F.);
#9321=ORIENTED_EDGE('',*,*,#6908,.T.);
#9322=ORIENTED_EDGE('',*,*,#6892,.F.);
#9323=ORIENTED_EDGE('',*,*,#6909,.T.);
#9324=ORIENTED_EDGE('',*,*,#6823,.T.);
#9325=ORIENTED_EDGE('',*,*,#6909,.F.);
#9326=ORIENTED_EDGE('',*,*,#6891,.F.);
#9327=ORIENTED_EDGE('',*,*,#6910,.F.);
#9328=ORIENTED_EDGE('',*,*,#6824,.F.);
#9329=ORIENTED_EDGE('',*,*,#6910,.T.);
#9330=ORIENTED_EDGE('',*,*,#6890,.F.);
#9331=ORIENTED_EDGE('',*,*,#6911,.T.);
#9332=ORIENTED_EDGE('',*,*,#6825,.T.);
#9333=ORIENTED_EDGE('',*,*,#6911,.F.);
#9334=ORIENTED_EDGE('',*,*,#6889,.F.);
#9335=ORIENTED_EDGE('',*,*,#6912,.F.);
#9336=ORIENTED_EDGE('',*,*,#6826,.F.);
#9337=ORIENTED_EDGE('',*,*,#6912,.T.);
#9338=ORIENTED_EDGE('',*,*,#6888,.F.);
#9339=ORIENTED_EDGE('',*,*,#6913,.T.);
#9340=ORIENTED_EDGE('',*,*,#6827,.T.);
#9341=ORIENTED_EDGE('',*,*,#6913,.F.);
#9342=ORIENTED_EDGE('',*,*,#6887,.F.);
#9343=ORIENTED_EDGE('',*,*,#6914,.F.);
#9344=ORIENTED_EDGE('',*,*,#6828,.F.);
#9345=ORIENTED_EDGE('',*,*,#6914,.T.);
#9346=ORIENTED_EDGE('',*,*,#6886,.F.);
#9347=ORIENTED_EDGE('',*,*,#6915,.T.);
#9348=ORIENTED_EDGE('',*,*,#6829,.T.);
#9349=ORIENTED_EDGE('',*,*,#6915,.F.);
#9350=ORIENTED_EDGE('',*,*,#6885,.F.);
#9351=ORIENTED_EDGE('',*,*,#6916,.F.);
#9352=ORIENTED_EDGE('',*,*,#6830,.F.);
#9353=ORIENTED_EDGE('',*,*,#6916,.T.);
#9354=ORIENTED_EDGE('',*,*,#6884,.F.);
#9355=ORIENTED_EDGE('',*,*,#6917,.T.);
#9356=ORIENTED_EDGE('',*,*,#6831,.T.);
#9357=ORIENTED_EDGE('',*,*,#6917,.F.);
#9358=ORIENTED_EDGE('',*,*,#6883,.F.);
#9359=ORIENTED_EDGE('',*,*,#6918,.F.);
#9360=ORIENTED_EDGE('',*,*,#6832,.F.);
#9361=ORIENTED_EDGE('',*,*,#6918,.T.);
#9362=ORIENTED_EDGE('',*,*,#6882,.F.);
#9363=ORIENTED_EDGE('',*,*,#6919,.T.);
#9364=ORIENTED_EDGE('',*,*,#6833,.T.);
#9365=ORIENTED_EDGE('',*,*,#6919,.F.);
#9366=ORIENTED_EDGE('',*,*,#6881,.F.);
#9367=ORIENTED_EDGE('',*,*,#6920,.F.);
#9368=ORIENTED_EDGE('',*,*,#6834,.F.);
#9369=ORIENTED_EDGE('',*,*,#6920,.T.);
#9370=ORIENTED_EDGE('',*,*,#6880,.F.);
#9371=ORIENTED_EDGE('',*,*,#6921,.T.);
#9372=ORIENTED_EDGE('',*,*,#6835,.T.);
#9373=ORIENTED_EDGE('',*,*,#6921,.F.);
#9374=ORIENTED_EDGE('',*,*,#6879,.F.);
#9375=ORIENTED_EDGE('',*,*,#6922,.F.);
#9376=ORIENTED_EDGE('',*,*,#6836,.F.);
#9377=ORIENTED_EDGE('',*,*,#6922,.T.);
#9378=ORIENTED_EDGE('',*,*,#6878,.F.);
#9379=ORIENTED_EDGE('',*,*,#6923,.T.);
#9380=ORIENTED_EDGE('',*,*,#6837,.T.);
#9381=ORIENTED_EDGE('',*,*,#6923,.F.);
#9382=ORIENTED_EDGE('',*,*,#6877,.F.);
#9383=ORIENTED_EDGE('',*,*,#6924,.F.);
#9384=ORIENTED_EDGE('',*,*,#6838,.F.);
#9385=ORIENTED_EDGE('',*,*,#6924,.T.);
#9386=ORIENTED_EDGE('',*,*,#6876,.F.);
#9387=ORIENTED_EDGE('',*,*,#6925,.T.);
#9388=ORIENTED_EDGE('',*,*,#6839,.T.);
#9389=ORIENTED_EDGE('',*,*,#6925,.F.);
#9390=ORIENTED_EDGE('',*,*,#6875,.F.);
#9391=ORIENTED_EDGE('',*,*,#6926,.F.);
#9392=ORIENTED_EDGE('',*,*,#6840,.F.);
#9393=ORIENTED_EDGE('',*,*,#6926,.T.);
#9394=ORIENTED_EDGE('',*,*,#6874,.F.);
#9395=ORIENTED_EDGE('',*,*,#6927,.T.);
#9396=ORIENTED_EDGE('',*,*,#6841,.T.);
#9397=ORIENTED_EDGE('',*,*,#6927,.F.);
#9398=ORIENTED_EDGE('',*,*,#6873,.F.);
#9399=ORIENTED_EDGE('',*,*,#6928,.F.);
#9400=ORIENTED_EDGE('',*,*,#6842,.F.);
#9401=ORIENTED_EDGE('',*,*,#6928,.T.);
#9402=ORIENTED_EDGE('',*,*,#6872,.F.);
#9403=ORIENTED_EDGE('',*,*,#6929,.T.);
#9404=ORIENTED_EDGE('',*,*,#6843,.T.);
#9405=ORIENTED_EDGE('',*,*,#6929,.F.);
#9406=ORIENTED_EDGE('',*,*,#6871,.F.);
#9407=ORIENTED_EDGE('',*,*,#6930,.F.);
#9408=ORIENTED_EDGE('',*,*,#6844,.F.);
#9409=ORIENTED_EDGE('',*,*,#6930,.T.);
#9410=ORIENTED_EDGE('',*,*,#6870,.F.);
#9411=ORIENTED_EDGE('',*,*,#6931,.T.);
#9412=ORIENTED_EDGE('',*,*,#6845,.T.);
#9413=ORIENTED_EDGE('',*,*,#6931,.F.);
#9414=ORIENTED_EDGE('',*,*,#6869,.F.);
#9415=ORIENTED_EDGE('',*,*,#6932,.F.);
#9416=ORIENTED_EDGE('',*,*,#6846,.F.);
#9417=ORIENTED_EDGE('',*,*,#6932,.T.);
#9418=ORIENTED_EDGE('',*,*,#6868,.F.);
#9419=ORIENTED_EDGE('',*,*,#6933,.T.);
#9420=ORIENTED_EDGE('',*,*,#6847,.T.);
#9421=ORIENTED_EDGE('',*,*,#6933,.F.);
#9422=ORIENTED_EDGE('',*,*,#6867,.F.);
#9423=ORIENTED_EDGE('',*,*,#6934,.F.);
#9424=ORIENTED_EDGE('',*,*,#6848,.F.);
#9425=ORIENTED_EDGE('',*,*,#6934,.T.);
#9426=ORIENTED_EDGE('',*,*,#6866,.F.);
#9427=ORIENTED_EDGE('',*,*,#6935,.T.);
#9428=ORIENTED_EDGE('',*,*,#6849,.T.);
#9429=ORIENTED_EDGE('',*,*,#6935,.F.);
#9430=ORIENTED_EDGE('',*,*,#6865,.F.);
#9431=ORIENTED_EDGE('',*,*,#6936,.F.);
#9432=ORIENTED_EDGE('',*,*,#6850,.F.);
#9433=ORIENTED_EDGE('',*,*,#6936,.T.);
#9434=ORIENTED_EDGE('',*,*,#6864,.F.);
#9435=ORIENTED_EDGE('',*,*,#6937,.T.);
#9436=ORIENTED_EDGE('',*,*,#6851,.T.);
#9437=ORIENTED_EDGE('',*,*,#6938,.F.);
#9438=ORIENTED_EDGE('',*,*,#6852,.F.);
#9439=ORIENTED_EDGE('',*,*,#6937,.F.);
#9440=ORIENTED_EDGE('',*,*,#6863,.F.);
#9441=ORIENTED_EDGE('',*,*,#6901,.T.);
#9442=ORIENTED_EDGE('',*,*,#6855,.T.);
#9443=ORIENTED_EDGE('',*,*,#6939,.T.);
#9444=ORIENTED_EDGE('',*,*,#6860,.F.);
#9445=ORIENTED_EDGE('',*,*,#6940,.F.);
#9446=ORIENTED_EDGE('',*,*,#6861,.F.);
#9447=ORIENTED_EDGE('',*,*,#6939,.F.);
#9448=ORIENTED_EDGE('',*,*,#6854,.F.);
#9449=ORIENTED_EDGE('',*,*,#6938,.T.);
#9450=ORIENTED_EDGE('',*,*,#6862,.F.);
#9451=ORIENTED_EDGE('',*,*,#6940,.T.);
#9452=ORIENTED_EDGE('',*,*,#6853,.T.);
#9453=ORIENTED_EDGE('',*,*,#6941,.F.);
#9454=ORIENTED_EDGE('',*,*,#6942,.T.);
#9455=ORIENTED_EDGE('',*,*,#6943,.T.);
#9456=ORIENTED_EDGE('',*,*,#6942,.F.);
#9457=ORIENTED_EDGE('',*,*,#6943,.F.);
#9458=ORIENTED_EDGE('',*,*,#6944,.F.);
#9459=ORIENTED_EDGE('',*,*,#6945,.F.);
#9460=ORIENTED_EDGE('',*,*,#6946,.T.);
#9461=ORIENTED_EDGE('',*,*,#6947,.T.);
#9462=ORIENTED_EDGE('',*,*,#6946,.F.);
#9463=ORIENTED_EDGE('',*,*,#6947,.F.);
#9464=ORIENTED_EDGE('',*,*,#6948,.F.);
#9465=ORIENTED_EDGE('',*,*,#6944,.T.);
#9466=ORIENTED_EDGE('',*,*,#6949,.T.);
#9467=ORIENTED_EDGE('',*,*,#6950,.F.);
#9468=ORIENTED_EDGE('',*,*,#6949,.F.);
#9469=ORIENTED_EDGE('',*,*,#6948,.T.);
#9470=ORIENTED_EDGE('',*,*,#6951,.T.);
#9471=ORIENTED_EDGE('',*,*,#6952,.F.);
#9472=ORIENTED_EDGE('',*,*,#6951,.F.);
#9473=ORIENTED_EDGE('',*,*,#6953,.F.);
#9474=ORIENTED_EDGE('',*,*,#6954,.T.);
#9475=ORIENTED_EDGE('',*,*,#6955,.F.);
#9476=ORIENTED_EDGE('',*,*,#6954,.F.);
#9477=ORIENTED_EDGE('',*,*,#6956,.F.);
#9478=ORIENTED_EDGE('',*,*,#6957,.T.);
#9479=ORIENTED_EDGE('',*,*,#6958,.F.);
#9480=ORIENTED_EDGE('',*,*,#6957,.F.);
#9481=ORIENTED_EDGE('',*,*,#6959,.F.);
#9482=ORIENTED_EDGE('',*,*,#6960,.T.);
#9483=ORIENTED_EDGE('',*,*,#6961,.F.);
#9484=ORIENTED_EDGE('',*,*,#6960,.F.);
#9485=ORIENTED_EDGE('',*,*,#6962,.F.);
#9486=ORIENTED_EDGE('',*,*,#6963,.T.);
#9487=ORIENTED_EDGE('',*,*,#6964,.F.);
#9488=ORIENTED_EDGE('',*,*,#6963,.F.);
#9489=ORIENTED_EDGE('',*,*,#6965,.T.);
#9490=ORIENTED_EDGE('',*,*,#6966,.T.);
#9491=ORIENTED_EDGE('',*,*,#6967,.F.);
#9492=ORIENTED_EDGE('',*,*,#6968,.F.);
#9493=ORIENTED_EDGE('',*,*,#6969,.T.);
#9494=ORIENTED_EDGE('',*,*,#6968,.T.);
#9495=ORIENTED_EDGE('',*,*,#6970,.F.);
#9496=ORIENTED_EDGE('',*,*,#6971,.F.);
#9497=ORIENTED_EDGE('',*,*,#6972,.T.);
#9498=ORIENTED_EDGE('',*,*,#6971,.T.);
#9499=ORIENTED_EDGE('',*,*,#6973,.F.);
#9500=ORIENTED_EDGE('',*,*,#6974,.F.);
#9501=ORIENTED_EDGE('',*,*,#6975,.T.);
#9502=ORIENTED_EDGE('',*,*,#6974,.T.);
#9503=ORIENTED_EDGE('',*,*,#6976,.F.);
#9504=ORIENTED_EDGE('',*,*,#6966,.F.);
#9505=ORIENTED_EDGE('',*,*,#6976,.T.);
#9506=ORIENTED_EDGE('',*,*,#6973,.T.);
#9507=ORIENTED_EDGE('',*,*,#6970,.T.);
#9508=ORIENTED_EDGE('',*,*,#6967,.T.);
#9509=ORIENTED_EDGE('',*,*,#6950,.T.);
#9510=ORIENTED_EDGE('',*,*,#6952,.T.);
#9511=ORIENTED_EDGE('',*,*,#6955,.T.);
#9512=ORIENTED_EDGE('',*,*,#6958,.T.);
#9513=ORIENTED_EDGE('',*,*,#6961,.T.);
#9514=ORIENTED_EDGE('',*,*,#6964,.T.);
#9515=ORIENTED_EDGE('',*,*,#6975,.F.);
#9516=ORIENTED_EDGE('',*,*,#6965,.F.);
#9517=ORIENTED_EDGE('',*,*,#6969,.F.);
#9518=ORIENTED_EDGE('',*,*,#6972,.F.);
#9519=ORIENTED_EDGE('',*,*,#6962,.T.);
#9520=ORIENTED_EDGE('',*,*,#6959,.T.);
#9521=ORIENTED_EDGE('',*,*,#6956,.T.);
#9522=ORIENTED_EDGE('',*,*,#6953,.T.);
#9523=ORIENTED_EDGE('',*,*,#6945,.T.);
#9524=ORIENTED_EDGE('',*,*,#6941,.T.);
#9525=ORIENTED_EDGE('',*,*,#6977,.F.);
#9526=ORIENTED_EDGE('',*,*,#6978,.T.);
#9527=ORIENTED_EDGE('',*,*,#6979,.T.);
#9528=ORIENTED_EDGE('',*,*,#6978,.F.);
#9529=ORIENTED_EDGE('',*,*,#6979,.F.);
#9530=ORIENTED_EDGE('',*,*,#6980,.F.);
#9531=ORIENTED_EDGE('',*,*,#6981,.T.);
#9532=ORIENTED_EDGE('',*,*,#6982,.T.);
#9533=ORIENTED_EDGE('',*,*,#6981,.F.);
#9534=ORIENTED_EDGE('',*,*,#6982,.F.);
#9535=ORIENTED_EDGE('',*,*,#6983,.F.);
#9536=ORIENTED_EDGE('',*,*,#6984,.F.);
#9537=ORIENTED_EDGE('',*,*,#6985,.F.);
#9538=ORIENTED_EDGE('',*,*,#6986,.F.);
#9539=ORIENTED_EDGE('',*,*,#6987,.F.);
#9540=ORIENTED_EDGE('',*,*,#6988,.F.);
#9541=ORIENTED_EDGE('',*,*,#6989,.F.);
#9542=ORIENTED_EDGE('',*,*,#6984,.T.);
#9543=ORIENTED_EDGE('',*,*,#6990,.F.);
#9544=ORIENTED_EDGE('',*,*,#6991,.T.);
#9545=ORIENTED_EDGE('',*,*,#6992,.F.);
#9546=ORIENTED_EDGE('',*,*,#6993,.F.);
#9547=ORIENTED_EDGE('',*,*,#6994,.F.);
#9548=ORIENTED_EDGE('',*,*,#6995,.F.);
#9549=ORIENTED_EDGE('',*,*,#6996,.F.);
#9550=ORIENTED_EDGE('',*,*,#6991,.F.);
#9551=ORIENTED_EDGE('',*,*,#6986,.T.);
#9552=ORIENTED_EDGE('',*,*,#6997,.T.);
#9553=ORIENTED_EDGE('',*,*,#6998,.T.);
#9554=ORIENTED_EDGE('',*,*,#6999,.T.);
#9555=ORIENTED_EDGE('',*,*,#7000,.F.);
#9556=ORIENTED_EDGE('',*,*,#7001,.F.);
#9557=ORIENTED_EDGE('',*,*,#6985,.T.);
#9558=ORIENTED_EDGE('',*,*,#6989,.T.);
#9559=ORIENTED_EDGE('',*,*,#7002,.T.);
#9560=ORIENTED_EDGE('',*,*,#6992,.T.);
#9561=ORIENTED_EDGE('',*,*,#6996,.T.);
#9562=ORIENTED_EDGE('',*,*,#7003,.T.);
#9563=ORIENTED_EDGE('',*,*,#7004,.F.);
#9564=ORIENTED_EDGE('',*,*,#6997,.F.);
#9565=ORIENTED_EDGE('',*,*,#7005,.F.);
#9566=ORIENTED_EDGE('',*,*,#7006,.T.);
#9567=ORIENTED_EDGE('',*,*,#7007,.F.);
#9568=ORIENTED_EDGE('',*,*,#7006,.F.);
#9569=ORIENTED_EDGE('',*,*,#7005,.T.);
#9570=ORIENTED_EDGE('',*,*,#7008,.F.);
#9571=ORIENTED_EDGE('',*,*,#7009,.T.);
#9572=ORIENTED_EDGE('',*,*,#7010,.F.);
#9573=ORIENTED_EDGE('',*,*,#7009,.F.);
#9574=ORIENTED_EDGE('',*,*,#7008,.T.);
#9575=ORIENTED_EDGE('',*,*,#7000,.T.);
#9576=ORIENTED_EDGE('',*,*,#7011,.T.);
#9577=ORIENTED_EDGE('',*,*,#7012,.T.);
#9578=ORIENTED_EDGE('',*,*,#7013,.T.);
#9579=ORIENTED_EDGE('',*,*,#7007,.T.);
#9580=ORIENTED_EDGE('',*,*,#7010,.T.);
#9581=ORIENTED_EDGE('',*,*,#7014,.T.);
#9582=ORIENTED_EDGE('',*,*,#7015,.T.);
#9583=ORIENTED_EDGE('',*,*,#7011,.F.);
#9584=ORIENTED_EDGE('',*,*,#6999,.F.);
#9585=ORIENTED_EDGE('',*,*,#7004,.T.);
#9586=ORIENTED_EDGE('',*,*,#7016,.F.);
#9587=ORIENTED_EDGE('',*,*,#7014,.F.);
#9588=ORIENTED_EDGE('',*,*,#6998,.F.);
#9589=ORIENTED_EDGE('',*,*,#6983,.T.);
#9590=ORIENTED_EDGE('',*,*,#7001,.T.);
#9591=ORIENTED_EDGE('',*,*,#7013,.F.);
#9592=ORIENTED_EDGE('',*,*,#7017,.F.);
#9593=ORIENTED_EDGE('',*,*,#6994,.T.);
#9594=ORIENTED_EDGE('',*,*,#6990,.T.);
#9595=ORIENTED_EDGE('',*,*,#7018,.T.);
#9596=ORIENTED_EDGE('',*,*,#6987,.T.);
#9597=ORIENTED_EDGE('',*,*,#6995,.T.);
#9598=ORIENTED_EDGE('',*,*,#7017,.T.);
#9599=ORIENTED_EDGE('',*,*,#7012,.F.);
#9600=ORIENTED_EDGE('',*,*,#7015,.F.);
#9601=ORIENTED_EDGE('',*,*,#7016,.T.);
#9602=ORIENTED_EDGE('',*,*,#7003,.F.);
#9603=ORIENTED_EDGE('',*,*,#6988,.T.);
#9604=ORIENTED_EDGE('',*,*,#7018,.F.);
#9605=ORIENTED_EDGE('',*,*,#6993,.T.);
#9606=ORIENTED_EDGE('',*,*,#7002,.F.);
#9607=ORIENTED_EDGE('',*,*,#6977,.T.);
#9608=ORIENTED_EDGE('',*,*,#6980,.T.);
#9609=ORIENTED_EDGE('',*,*,#7019,.T.);
#9610=ORIENTED_EDGE('',*,*,#7020,.T.);
#9611=ORIENTED_EDGE('',*,*,#7021,.F.);
#9612=ORIENTED_EDGE('',*,*,#7022,.F.);
#9613=ORIENTED_EDGE('',*,*,#7023,.T.);
#9614=ORIENTED_EDGE('',*,*,#7022,.T.);
#9615=ORIENTED_EDGE('',*,*,#7024,.F.);
#9616=ORIENTED_EDGE('',*,*,#7025,.F.);
#9617=ORIENTED_EDGE('',*,*,#7026,.T.);
#9618=ORIENTED_EDGE('',*,*,#7025,.T.);
#9619=ORIENTED_EDGE('',*,*,#7027,.F.);
#9620=ORIENTED_EDGE('',*,*,#7028,.F.);
#9621=ORIENTED_EDGE('',*,*,#7029,.T.);
#9622=ORIENTED_EDGE('',*,*,#7028,.T.);
#9623=ORIENTED_EDGE('',*,*,#7030,.F.);
#9624=ORIENTED_EDGE('',*,*,#7020,.F.);
#9625=ORIENTED_EDGE('',*,*,#7030,.T.);
#9626=ORIENTED_EDGE('',*,*,#7027,.T.);
#9627=ORIENTED_EDGE('',*,*,#7024,.T.);
#9628=ORIENTED_EDGE('',*,*,#7021,.T.);
#9629=ORIENTED_EDGE('',*,*,#7029,.F.);
#9630=ORIENTED_EDGE('',*,*,#7019,.F.);
#9631=ORIENTED_EDGE('',*,*,#7023,.F.);
#9632=ORIENTED_EDGE('',*,*,#7026,.F.);
#9633=ORIENTED_EDGE('',*,*,#7031,.F.);
#9634=ORIENTED_EDGE('',*,*,#7032,.T.);
#9635=ORIENTED_EDGE('',*,*,#7033,.F.);
#9636=ORIENTED_EDGE('',*,*,#7034,.F.);
#9637=ORIENTED_EDGE('',*,*,#7035,.T.);
#9638=ORIENTED_EDGE('',*,*,#7036,.F.);
#9639=ORIENTED_EDGE('',*,*,#7035,.F.);
#9640=ORIENTED_EDGE('',*,*,#7037,.F.);
#9641=ORIENTED_EDGE('',*,*,#7038,.F.);
#9642=ORIENTED_EDGE('',*,*,#7032,.F.);
#9643=ORIENTED_EDGE('',*,*,#7039,.F.);
#9644=ORIENTED_EDGE('',*,*,#7040,.T.);
#9645=ORIENTED_EDGE('',*,*,#7041,.F.);
#9646=ORIENTED_EDGE('',*,*,#7042,.F.);
#9647=ORIENTED_EDGE('',*,*,#7043,.T.);
#9648=ORIENTED_EDGE('',*,*,#7044,.F.);
#9649=ORIENTED_EDGE('',*,*,#7043,.F.);
#9650=ORIENTED_EDGE('',*,*,#7045,.F.);
#9651=ORIENTED_EDGE('',*,*,#7046,.F.);
#9652=ORIENTED_EDGE('',*,*,#7040,.F.);
#9653=ORIENTED_EDGE('',*,*,#7047,.F.);
#9654=ORIENTED_EDGE('',*,*,#7048,.T.);
#9655=ORIENTED_EDGE('',*,*,#7049,.F.);
#9656=ORIENTED_EDGE('',*,*,#7050,.F.);
#9657=ORIENTED_EDGE('',*,*,#7051,.T.);
#9658=ORIENTED_EDGE('',*,*,#7052,.F.);
#9659=ORIENTED_EDGE('',*,*,#7051,.F.);
#9660=ORIENTED_EDGE('',*,*,#7053,.F.);
#9661=ORIENTED_EDGE('',*,*,#7054,.F.);
#9662=ORIENTED_EDGE('',*,*,#7048,.F.);
#9663=ORIENTED_EDGE('',*,*,#7055,.F.);
#9664=ORIENTED_EDGE('',*,*,#7056,.T.);
#9665=ORIENTED_EDGE('',*,*,#7057,.F.);
#9666=ORIENTED_EDGE('',*,*,#7058,.F.);
#9667=ORIENTED_EDGE('',*,*,#7059,.T.);
#9668=ORIENTED_EDGE('',*,*,#7060,.F.);
#9669=ORIENTED_EDGE('',*,*,#7059,.F.);
#9670=ORIENTED_EDGE('',*,*,#7061,.F.);
#9671=ORIENTED_EDGE('',*,*,#7062,.F.);
#9672=ORIENTED_EDGE('',*,*,#7056,.F.);
#9673=ORIENTED_EDGE('',*,*,#7033,.T.);
#9674=ORIENTED_EDGE('',*,*,#7031,.T.);
#9675=ORIENTED_EDGE('',*,*,#7038,.T.);
#9676=ORIENTED_EDGE('',*,*,#7063,.T.);
#9677=ORIENTED_EDGE('',*,*,#7049,.T.);
#9678=ORIENTED_EDGE('',*,*,#7047,.T.);
#9679=ORIENTED_EDGE('',*,*,#7054,.T.);
#9680=ORIENTED_EDGE('',*,*,#7064,.T.);
#9681=ORIENTED_EDGE('',*,*,#7065,.F.);
#9682=ORIENTED_EDGE('',*,*,#7066,.T.);
#9683=ORIENTED_EDGE('',*,*,#7067,.F.);
#9684=ORIENTED_EDGE('',*,*,#7068,.T.);
#9685=ORIENTED_EDGE('',*,*,#7041,.T.);
#9686=ORIENTED_EDGE('',*,*,#7039,.T.);
#9687=ORIENTED_EDGE('',*,*,#7046,.T.);
#9688=ORIENTED_EDGE('',*,*,#7069,.T.);
#9689=ORIENTED_EDGE('',*,*,#7057,.T.);
#9690=ORIENTED_EDGE('',*,*,#7055,.T.);
#9691=ORIENTED_EDGE('',*,*,#7062,.T.);
#9692=ORIENTED_EDGE('',*,*,#7070,.T.);
#9693=ORIENTED_EDGE('',*,*,#7071,.F.);
#9694=ORIENTED_EDGE('',*,*,#7072,.F.);
#9695=ORIENTED_EDGE('',*,*,#7073,.F.);
#9696=ORIENTED_EDGE('',*,*,#7074,.T.);
#9697=ORIENTED_EDGE('',*,*,#7065,.T.);
#9698=ORIENTED_EDGE('',*,*,#7075,.T.);
#9699=ORIENTED_EDGE('',*,*,#7076,.T.);
#9700=ORIENTED_EDGE('',*,*,#7077,.T.);
#9701=ORIENTED_EDGE('',*,*,#7078,.T.);
#9702=ORIENTED_EDGE('',*,*,#7079,.T.);
#9703=ORIENTED_EDGE('',*,*,#7073,.T.);
#9704=ORIENTED_EDGE('',*,*,#7080,.T.);
#9705=ORIENTED_EDGE('',*,*,#7081,.T.);
#9706=ORIENTED_EDGE('',*,*,#7082,.T.);
#9707=ORIENTED_EDGE('',*,*,#7083,.T.);
#9708=ORIENTED_EDGE('',*,*,#7084,.T.);
#9709=ORIENTED_EDGE('',*,*,#7037,.T.);
#9710=ORIENTED_EDGE('',*,*,#7034,.T.);
#9711=ORIENTED_EDGE('',*,*,#7068,.F.);
#9712=ORIENTED_EDGE('',*,*,#7085,.F.);
#9713=ORIENTED_EDGE('',*,*,#7086,.F.);
#9714=ORIENTED_EDGE('',*,*,#7075,.F.);
#9715=ORIENTED_EDGE('',*,*,#7064,.F.);
#9716=ORIENTED_EDGE('',*,*,#7053,.T.);
#9717=ORIENTED_EDGE('',*,*,#7050,.T.);
#9718=ORIENTED_EDGE('',*,*,#7063,.F.);
#9719=ORIENTED_EDGE('',*,*,#7086,.T.);
#9720=ORIENTED_EDGE('',*,*,#7087,.F.);
#9721=ORIENTED_EDGE('',*,*,#7088,.F.);
#9722=ORIENTED_EDGE('',*,*,#7076,.F.);
#9723=ORIENTED_EDGE('',*,*,#7088,.T.);
#9724=ORIENTED_EDGE('',*,*,#7089,.F.);
#9725=ORIENTED_EDGE('',*,*,#7090,.F.);
#9726=ORIENTED_EDGE('',*,*,#7077,.F.);
#9727=ORIENTED_EDGE('',*,*,#7036,.T.);
#9728=ORIENTED_EDGE('',*,*,#7044,.T.);
#9729=ORIENTED_EDGE('',*,*,#7052,.T.);
#9730=ORIENTED_EDGE('',*,*,#7060,.T.);
#9731=ORIENTED_EDGE('',*,*,#7090,.T.);
#9732=ORIENTED_EDGE('',*,*,#7091,.F.);
#9733=ORIENTED_EDGE('',*,*,#7092,.F.);
#9734=ORIENTED_EDGE('',*,*,#7078,.F.);
#9735=ORIENTED_EDGE('',*,*,#7045,.T.);
#9736=ORIENTED_EDGE('',*,*,#7042,.T.);
#9737=ORIENTED_EDGE('',*,*,#7074,.F.);
#9738=ORIENTED_EDGE('',*,*,#7079,.F.);
#9739=ORIENTED_EDGE('',*,*,#7092,.T.);
#9740=ORIENTED_EDGE('',*,*,#7093,.F.);
#9741=ORIENTED_EDGE('',*,*,#7070,.F.);
#9742=ORIENTED_EDGE('',*,*,#7061,.T.);
#9743=ORIENTED_EDGE('',*,*,#7058,.T.);
#9744=ORIENTED_EDGE('',*,*,#7069,.F.);
#9745=ORIENTED_EDGE('',*,*,#7072,.T.);
#9746=ORIENTED_EDGE('',*,*,#7094,.F.);
#9747=ORIENTED_EDGE('',*,*,#7095,.F.);
#9748=ORIENTED_EDGE('',*,*,#7080,.F.);
#9749=ORIENTED_EDGE('',*,*,#7095,.T.);
#9750=ORIENTED_EDGE('',*,*,#7096,.F.);
#9751=ORIENTED_EDGE('',*,*,#7097,.F.);
#9752=ORIENTED_EDGE('',*,*,#7081,.F.);
#9753=ORIENTED_EDGE('',*,*,#7097,.T.);
#9754=ORIENTED_EDGE('',*,*,#7098,.F.);
#9755=ORIENTED_EDGE('',*,*,#7099,.F.);
#9756=ORIENTED_EDGE('',*,*,#7082,.F.);
#9757=ORIENTED_EDGE('',*,*,#7099,.T.);
#9758=ORIENTED_EDGE('',*,*,#7100,.F.);
#9759=ORIENTED_EDGE('',*,*,#7101,.F.);
#9760=ORIENTED_EDGE('',*,*,#7083,.F.);
#9761=ORIENTED_EDGE('',*,*,#7101,.T.);
#9762=ORIENTED_EDGE('',*,*,#7102,.F.);
#9763=ORIENTED_EDGE('',*,*,#7066,.F.);
#9764=ORIENTED_EDGE('',*,*,#7084,.F.);
#9765=ORIENTED_EDGE('',*,*,#7067,.T.);
#9766=ORIENTED_EDGE('',*,*,#7102,.T.);
#9767=ORIENTED_EDGE('',*,*,#7100,.T.);
#9768=ORIENTED_EDGE('',*,*,#7098,.T.);
#9769=ORIENTED_EDGE('',*,*,#7096,.T.);
#9770=ORIENTED_EDGE('',*,*,#7094,.T.);
#9771=ORIENTED_EDGE('',*,*,#7071,.T.);
#9772=ORIENTED_EDGE('',*,*,#7093,.T.);
#9773=ORIENTED_EDGE('',*,*,#7091,.T.);
#9774=ORIENTED_EDGE('',*,*,#7089,.T.);
#9775=ORIENTED_EDGE('',*,*,#7087,.T.);
#9776=ORIENTED_EDGE('',*,*,#7085,.T.);
#9777=ORIENTED_EDGE('',*,*,#7103,.T.);
#9778=ORIENTED_EDGE('',*,*,#7104,.T.);
#9779=ORIENTED_EDGE('',*,*,#7105,.F.);
#9780=ORIENTED_EDGE('',*,*,#7106,.F.);
#9781=ORIENTED_EDGE('',*,*,#7107,.T.);
#9782=ORIENTED_EDGE('',*,*,#7106,.T.);
#9783=ORIENTED_EDGE('',*,*,#7108,.F.);
#9784=ORIENTED_EDGE('',*,*,#7109,.F.);
#9785=ORIENTED_EDGE('',*,*,#7110,.T.);
#9786=ORIENTED_EDGE('',*,*,#7109,.T.);
#9787=ORIENTED_EDGE('',*,*,#7111,.F.);
#9788=ORIENTED_EDGE('',*,*,#7112,.F.);
#9789=ORIENTED_EDGE('',*,*,#7113,.T.);
#9790=ORIENTED_EDGE('',*,*,#7112,.T.);
#9791=ORIENTED_EDGE('',*,*,#7114,.F.);
#9792=ORIENTED_EDGE('',*,*,#7115,.F.);
#9793=ORIENTED_EDGE('',*,*,#7116,.T.);
#9794=ORIENTED_EDGE('',*,*,#7115,.T.);
#9795=ORIENTED_EDGE('',*,*,#7117,.F.);
#9796=ORIENTED_EDGE('',*,*,#7118,.F.);
#9797=ORIENTED_EDGE('',*,*,#7119,.T.);
#9798=ORIENTED_EDGE('',*,*,#7118,.T.);
#9799=ORIENTED_EDGE('',*,*,#7120,.F.);
#9800=ORIENTED_EDGE('',*,*,#7121,.F.);
#9801=ORIENTED_EDGE('',*,*,#7122,.T.);
#9802=ORIENTED_EDGE('',*,*,#7121,.T.);
#9803=ORIENTED_EDGE('',*,*,#7123,.F.);
#9804=ORIENTED_EDGE('',*,*,#7124,.F.);
#9805=ORIENTED_EDGE('',*,*,#7125,.T.);
#9806=ORIENTED_EDGE('',*,*,#7124,.T.);
#9807=ORIENTED_EDGE('',*,*,#7126,.F.);
#9808=ORIENTED_EDGE('',*,*,#7104,.F.);
#9809=ORIENTED_EDGE('',*,*,#7126,.T.);
#9810=ORIENTED_EDGE('',*,*,#7123,.T.);
#9811=ORIENTED_EDGE('',*,*,#7120,.T.);
#9812=ORIENTED_EDGE('',*,*,#7117,.T.);
#9813=ORIENTED_EDGE('',*,*,#7114,.T.);
#9814=ORIENTED_EDGE('',*,*,#7111,.T.);
#9815=ORIENTED_EDGE('',*,*,#7108,.T.);
#9816=ORIENTED_EDGE('',*,*,#7105,.T.);
#9817=ORIENTED_EDGE('',*,*,#7125,.F.);
#9818=ORIENTED_EDGE('',*,*,#7103,.F.);
#9819=ORIENTED_EDGE('',*,*,#7107,.F.);
#9820=ORIENTED_EDGE('',*,*,#7110,.F.);
#9821=ORIENTED_EDGE('',*,*,#7113,.F.);
#9822=ORIENTED_EDGE('',*,*,#7116,.F.);
#9823=ORIENTED_EDGE('',*,*,#7119,.F.);
#9824=ORIENTED_EDGE('',*,*,#7122,.F.);
#9825=ORIENTED_EDGE('',*,*,#7127,.F.);
#9826=ORIENTED_EDGE('',*,*,#7128,.T.);
#9827=ORIENTED_EDGE('',*,*,#7129,.F.);
#9828=ORIENTED_EDGE('',*,*,#7130,.F.);
#9829=ORIENTED_EDGE('',*,*,#7131,.F.);
#9830=ORIENTED_EDGE('',*,*,#7130,.T.);
#9831=ORIENTED_EDGE('',*,*,#7132,.F.);
#9832=ORIENTED_EDGE('',*,*,#7133,.F.);
#9833=ORIENTED_EDGE('',*,*,#7134,.F.);
#9834=ORIENTED_EDGE('',*,*,#7133,.T.);
#9835=ORIENTED_EDGE('',*,*,#7135,.F.);
#9836=ORIENTED_EDGE('',*,*,#7136,.F.);
#9837=ORIENTED_EDGE('',*,*,#7137,.F.);
#9838=ORIENTED_EDGE('',*,*,#7136,.T.);
#9839=ORIENTED_EDGE('',*,*,#7138,.F.);
#9840=ORIENTED_EDGE('',*,*,#7139,.F.);
#9841=ORIENTED_EDGE('',*,*,#7140,.F.);
#9842=ORIENTED_EDGE('',*,*,#7139,.T.);
#9843=ORIENTED_EDGE('',*,*,#7141,.F.);
#9844=ORIENTED_EDGE('',*,*,#7142,.F.);
#9845=ORIENTED_EDGE('',*,*,#7143,.F.);
#9846=ORIENTED_EDGE('',*,*,#7142,.T.);
#9847=ORIENTED_EDGE('',*,*,#7144,.F.);
#9848=ORIENTED_EDGE('',*,*,#7145,.F.);
#9849=ORIENTED_EDGE('',*,*,#7146,.F.);
#9850=ORIENTED_EDGE('',*,*,#7145,.T.);
#9851=ORIENTED_EDGE('',*,*,#7147,.F.);
#9852=ORIENTED_EDGE('',*,*,#7148,.F.);
#9853=ORIENTED_EDGE('',*,*,#7149,.F.);
#9854=ORIENTED_EDGE('',*,*,#7148,.T.);
#9855=ORIENTED_EDGE('',*,*,#7150,.F.);
#9856=ORIENTED_EDGE('',*,*,#7128,.F.);
#9857=ORIENTED_EDGE('',*,*,#7149,.T.);
#9858=ORIENTED_EDGE('',*,*,#7127,.T.);
#9859=ORIENTED_EDGE('',*,*,#7131,.T.);
#9860=ORIENTED_EDGE('',*,*,#7134,.T.);
#9861=ORIENTED_EDGE('',*,*,#7137,.T.);
#9862=ORIENTED_EDGE('',*,*,#7140,.T.);
#9863=ORIENTED_EDGE('',*,*,#7143,.T.);
#9864=ORIENTED_EDGE('',*,*,#7146,.T.);
#9865=ORIENTED_EDGE('',*,*,#7150,.T.);
#9866=ORIENTED_EDGE('',*,*,#7147,.T.);
#9867=ORIENTED_EDGE('',*,*,#7144,.T.);
#9868=ORIENTED_EDGE('',*,*,#7141,.T.);
#9869=ORIENTED_EDGE('',*,*,#7138,.T.);
#9870=ORIENTED_EDGE('',*,*,#7135,.T.);
#9871=ORIENTED_EDGE('',*,*,#7132,.T.);
#9872=ORIENTED_EDGE('',*,*,#7129,.T.);
#9873=ORIENTED_EDGE('',*,*,#7151,.T.);
#9874=ORIENTED_EDGE('',*,*,#7152,.T.);
#9875=ORIENTED_EDGE('',*,*,#7153,.T.);
#9876=ORIENTED_EDGE('',*,*,#7152,.F.);
#9877=ORIENTED_EDGE('',*,*,#7153,.F.);
#9878=ORIENTED_EDGE('',*,*,#7154,.T.);
#9879=ORIENTED_EDGE('',*,*,#7155,.T.);
#9880=ORIENTED_EDGE('',*,*,#7154,.F.);
#9881=ORIENTED_EDGE('',*,*,#7156,.T.);
#9882=ORIENTED_EDGE('',*,*,#7151,.F.);
#9883=ORIENTED_EDGE('',*,*,#7156,.F.);
#9884=ORIENTED_EDGE('',*,*,#7157,.T.);
#9885=ORIENTED_EDGE('',*,*,#7158,.T.);
#9886=ORIENTED_EDGE('',*,*,#7157,.F.);
#9887=ORIENTED_EDGE('',*,*,#7158,.F.);
#9888=ORIENTED_EDGE('',*,*,#7155,.F.);
#9889=ORIENTED_EDGE('',*,*,#7159,.F.);
#9890=ORIENTED_EDGE('',*,*,#7160,.F.);
#9891=ORIENTED_EDGE('',*,*,#7161,.T.);
#9892=ORIENTED_EDGE('',*,*,#7159,.T.);
#9893=ORIENTED_EDGE('',*,*,#7161,.F.);
#9894=ORIENTED_EDGE('',*,*,#7162,.F.);
#9895=ORIENTED_EDGE('',*,*,#7163,.T.);
#9896=ORIENTED_EDGE('',*,*,#7160,.T.);
#9897=ORIENTED_EDGE('',*,*,#7163,.F.);
#9898=ORIENTED_EDGE('',*,*,#7164,.F.);
#9899=ORIENTED_EDGE('',*,*,#7165,.T.);
#9900=ORIENTED_EDGE('',*,*,#7162,.T.);
#9901=ORIENTED_EDGE('',*,*,#7165,.F.);
#9902=ORIENTED_EDGE('',*,*,#7164,.T.);
#9903=ORIENTED_EDGE('',*,*,#7166,.F.);
#9904=ORIENTED_EDGE('',*,*,#7167,.F.);
#9905=ORIENTED_EDGE('',*,*,#7168,.T.);
#9906=ORIENTED_EDGE('',*,*,#7166,.T.);
#9907=ORIENTED_EDGE('',*,*,#7168,.F.);
#9908=ORIENTED_EDGE('',*,*,#7169,.F.);
#9909=ORIENTED_EDGE('',*,*,#7170,.T.);
#9910=ORIENTED_EDGE('',*,*,#7167,.T.);
#9911=ORIENTED_EDGE('',*,*,#7170,.F.);
#9912=ORIENTED_EDGE('',*,*,#7171,.F.);
#9913=ORIENTED_EDGE('',*,*,#7172,.T.);
#9914=ORIENTED_EDGE('',*,*,#7169,.T.);
#9915=ORIENTED_EDGE('',*,*,#7172,.F.);
#9916=ORIENTED_EDGE('',*,*,#7171,.T.);
#9917=ORIENTED_EDGE('',*,*,#7173,.T.);
#9918=ORIENTED_EDGE('',*,*,#7174,.T.);
#9919=ORIENTED_EDGE('',*,*,#7175,.T.);
#9920=ORIENTED_EDGE('',*,*,#7176,.F.);
#9921=ORIENTED_EDGE('',*,*,#7177,.T.);
#9922=ORIENTED_EDGE('',*,*,#7178,.T.);
#9923=ORIENTED_EDGE('',*,*,#7179,.T.);
#9924=ORIENTED_EDGE('',*,*,#7174,.F.);
#9925=ORIENTED_EDGE('',*,*,#7180,.T.);
#9926=ORIENTED_EDGE('',*,*,#7181,.T.);
#9927=ORIENTED_EDGE('',*,*,#7182,.T.);
#9928=ORIENTED_EDGE('',*,*,#7178,.F.);
#9929=ORIENTED_EDGE('',*,*,#7183,.T.);
#9930=ORIENTED_EDGE('',*,*,#7184,.T.);
#9931=ORIENTED_EDGE('',*,*,#7185,.T.);
#9932=ORIENTED_EDGE('',*,*,#7181,.F.);
#9933=ORIENTED_EDGE('',*,*,#7186,.T.);
#9934=ORIENTED_EDGE('',*,*,#7187,.T.);
#9935=ORIENTED_EDGE('',*,*,#7188,.T.);
#9936=ORIENTED_EDGE('',*,*,#7184,.F.);
#9937=ORIENTED_EDGE('',*,*,#7189,.T.);
#9938=ORIENTED_EDGE('',*,*,#7176,.T.);
#9939=ORIENTED_EDGE('',*,*,#7190,.T.);
#9940=ORIENTED_EDGE('',*,*,#7187,.F.);
#9941=ORIENTED_EDGE('',*,*,#7189,.F.);
#9942=ORIENTED_EDGE('',*,*,#7186,.F.);
#9943=ORIENTED_EDGE('',*,*,#7183,.F.);
#9944=ORIENTED_EDGE('',*,*,#7180,.F.);
#9945=ORIENTED_EDGE('',*,*,#7177,.F.);
#9946=ORIENTED_EDGE('',*,*,#7173,.F.);
#9947=ORIENTED_EDGE('',*,*,#7190,.F.);
#9948=ORIENTED_EDGE('',*,*,#7175,.F.);
#9949=ORIENTED_EDGE('',*,*,#7179,.F.);
#9950=ORIENTED_EDGE('',*,*,#7182,.F.);
#9951=ORIENTED_EDGE('',*,*,#7185,.F.);
#9952=ORIENTED_EDGE('',*,*,#7188,.F.);
#9953=ORIENTED_EDGE('',*,*,#7191,.T.);
#9954=ORIENTED_EDGE('',*,*,#7192,.T.);
#9955=ORIENTED_EDGE('',*,*,#7193,.T.);
#9956=ORIENTED_EDGE('',*,*,#7194,.F.);
#9957=ORIENTED_EDGE('',*,*,#7195,.T.);
#9958=ORIENTED_EDGE('',*,*,#7196,.T.);
#9959=ORIENTED_EDGE('',*,*,#7197,.T.);
#9960=ORIENTED_EDGE('',*,*,#7192,.F.);
#9961=ORIENTED_EDGE('',*,*,#7198,.T.);
#9962=ORIENTED_EDGE('',*,*,#7199,.T.);
#9963=ORIENTED_EDGE('',*,*,#7200,.T.);
#9964=ORIENTED_EDGE('',*,*,#7196,.F.);
#9965=ORIENTED_EDGE('',*,*,#7201,.T.);
#9966=ORIENTED_EDGE('',*,*,#7202,.T.);
#9967=ORIENTED_EDGE('',*,*,#7203,.T.);
#9968=ORIENTED_EDGE('',*,*,#7199,.F.);
#9969=ORIENTED_EDGE('',*,*,#7204,.T.);
#9970=ORIENTED_EDGE('',*,*,#7205,.T.);
#9971=ORIENTED_EDGE('',*,*,#7206,.T.);
#9972=ORIENTED_EDGE('',*,*,#7202,.F.);
#9973=ORIENTED_EDGE('',*,*,#7207,.T.);
#9974=ORIENTED_EDGE('',*,*,#7194,.T.);
#9975=ORIENTED_EDGE('',*,*,#7208,.T.);
#9976=ORIENTED_EDGE('',*,*,#7205,.F.);
#9977=ORIENTED_EDGE('',*,*,#7207,.F.);
#9978=ORIENTED_EDGE('',*,*,#7204,.F.);
#9979=ORIENTED_EDGE('',*,*,#7201,.F.);
#9980=ORIENTED_EDGE('',*,*,#7198,.F.);
#9981=ORIENTED_EDGE('',*,*,#7195,.F.);
#9982=ORIENTED_EDGE('',*,*,#7191,.F.);
#9983=ORIENTED_EDGE('',*,*,#7208,.F.);
#9984=ORIENTED_EDGE('',*,*,#7193,.F.);
#9985=ORIENTED_EDGE('',*,*,#7197,.F.);
#9986=ORIENTED_EDGE('',*,*,#7200,.F.);
#9987=ORIENTED_EDGE('',*,*,#7203,.F.);
#9988=ORIENTED_EDGE('',*,*,#7206,.F.);
#9989=ORIENTED_EDGE('',*,*,#7209,.F.);
#9990=ORIENTED_EDGE('',*,*,#7210,.F.);
#9991=ORIENTED_EDGE('',*,*,#7211,.F.);
#9992=ORIENTED_EDGE('',*,*,#7212,.T.);
#9993=ORIENTED_EDGE('',*,*,#7210,.T.);
#9994=ORIENTED_EDGE('',*,*,#7212,.F.);
#9995=ORIENTED_EDGE('',*,*,#7213,.F.);
#9996=ORIENTED_EDGE('',*,*,#7214,.T.);
#9997=ORIENTED_EDGE('',*,*,#7211,.T.);
#9998=ORIENTED_EDGE('',*,*,#7214,.F.);
#9999=ORIENTED_EDGE('',*,*,#7215,.F.);
#10000=ORIENTED_EDGE('',*,*,#7216,.T.);
#10001=ORIENTED_EDGE('',*,*,#7213,.T.);
#10002=ORIENTED_EDGE('',*,*,#7216,.F.);
#10003=ORIENTED_EDGE('',*,*,#7215,.T.);
#10004=ORIENTED_EDGE('',*,*,#7217,.F.);
#10005=ORIENTED_EDGE('',*,*,#7218,.F.);
#10006=ORIENTED_EDGE('',*,*,#7219,.T.);
#10007=ORIENTED_EDGE('',*,*,#7217,.T.);
#10008=ORIENTED_EDGE('',*,*,#7219,.F.);
#10009=ORIENTED_EDGE('',*,*,#7209,.T.);
#10010=ORIENTED_EDGE('',*,*,#7220,.T.);
#10011=ORIENTED_EDGE('',*,*,#7218,.T.);
#10012=ORIENTED_EDGE('',*,*,#7220,.F.);
#10013=ORIENTED_EDGE('',*,*,#7221,.F.);
#10014=ORIENTED_EDGE('',*,*,#7222,.F.);
#10015=ORIENTED_EDGE('',*,*,#7223,.T.);
#10016=ORIENTED_EDGE('',*,*,#7221,.T.);
#10017=ORIENTED_EDGE('',*,*,#7223,.F.);
#10018=ORIENTED_EDGE('',*,*,#7224,.F.);
#10019=ORIENTED_EDGE('',*,*,#7225,.T.);
#10020=ORIENTED_EDGE('',*,*,#7222,.T.);
#10021=ORIENTED_EDGE('',*,*,#7225,.F.);
#10022=ORIENTED_EDGE('',*,*,#7226,.F.);
#10023=ORIENTED_EDGE('',*,*,#7227,.T.);
#10024=ORIENTED_EDGE('',*,*,#7224,.T.);
#10025=ORIENTED_EDGE('',*,*,#7227,.F.);
#10026=ORIENTED_EDGE('',*,*,#7226,.T.);
#10027=ORIENTED_EDGE('',*,*,#7228,.F.);
#10028=ORIENTED_EDGE('',*,*,#7229,.F.);
#10029=ORIENTED_EDGE('',*,*,#7230,.T.);
#10030=ORIENTED_EDGE('',*,*,#7228,.T.);
#10031=ORIENTED_EDGE('',*,*,#7230,.F.);
#10032=ORIENTED_EDGE('',*,*,#7231,.F.);
#10033=ORIENTED_EDGE('',*,*,#7232,.T.);
#10034=ORIENTED_EDGE('',*,*,#7229,.T.);
#10035=ORIENTED_EDGE('',*,*,#7232,.F.);
#10036=ORIENTED_EDGE('',*,*,#7233,.F.);
#10037=ORIENTED_EDGE('',*,*,#7234,.T.);
#10038=ORIENTED_EDGE('',*,*,#7231,.T.);
#10039=ORIENTED_EDGE('',*,*,#7234,.F.);
#10040=ORIENTED_EDGE('',*,*,#7233,.T.);
#10041=ORIENTED_EDGE('',*,*,#7235,.T.);
#10042=ORIENTED_EDGE('',*,*,#7236,.T.);
#10043=ORIENTED_EDGE('',*,*,#7237,.T.);
#10044=ORIENTED_EDGE('',*,*,#7238,.F.);
#10045=ORIENTED_EDGE('',*,*,#7239,.T.);
#10046=ORIENTED_EDGE('',*,*,#7240,.T.);
#10047=ORIENTED_EDGE('',*,*,#7241,.T.);
#10048=ORIENTED_EDGE('',*,*,#7236,.F.);
#10049=ORIENTED_EDGE('',*,*,#7242,.T.);
#10050=ORIENTED_EDGE('',*,*,#7243,.T.);
#10051=ORIENTED_EDGE('',*,*,#7244,.T.);
#10052=ORIENTED_EDGE('',*,*,#7240,.F.);
#10053=ORIENTED_EDGE('',*,*,#7245,.T.);
#10054=ORIENTED_EDGE('',*,*,#7246,.T.);
#10055=ORIENTED_EDGE('',*,*,#7247,.T.);
#10056=ORIENTED_EDGE('',*,*,#7243,.F.);
#10057=ORIENTED_EDGE('',*,*,#7248,.T.);
#10058=ORIENTED_EDGE('',*,*,#7249,.T.);
#10059=ORIENTED_EDGE('',*,*,#7250,.T.);
#10060=ORIENTED_EDGE('',*,*,#7246,.F.);
#10061=ORIENTED_EDGE('',*,*,#7251,.T.);
#10062=ORIENTED_EDGE('',*,*,#7238,.T.);
#10063=ORIENTED_EDGE('',*,*,#7252,.T.);
#10064=ORIENTED_EDGE('',*,*,#7249,.F.);
#10065=ORIENTED_EDGE('',*,*,#7251,.F.);
#10066=ORIENTED_EDGE('',*,*,#7248,.F.);
#10067=ORIENTED_EDGE('',*,*,#7245,.F.);
#10068=ORIENTED_EDGE('',*,*,#7242,.F.);
#10069=ORIENTED_EDGE('',*,*,#7239,.F.);
#10070=ORIENTED_EDGE('',*,*,#7235,.F.);
#10071=ORIENTED_EDGE('',*,*,#7252,.F.);
#10072=ORIENTED_EDGE('',*,*,#7237,.F.);
#10073=ORIENTED_EDGE('',*,*,#7241,.F.);
#10074=ORIENTED_EDGE('',*,*,#7244,.F.);
#10075=ORIENTED_EDGE('',*,*,#7247,.F.);
#10076=ORIENTED_EDGE('',*,*,#7250,.F.);
#10077=CYLINDRICAL_SURFACE('',#11493,0.164999999999999);
#10078=CYLINDRICAL_SURFACE('',#11497,0.164999999999999);
#10079=CYLINDRICAL_SURFACE('',#11501,0.165);
#10080=CYLINDRICAL_SURFACE('',#11505,0.165);
#10081=CYLINDRICAL_SURFACE('',#11509,0.164999999999999);
#10082=CYLINDRICAL_SURFACE('',#11513,0.164999999999999);
#10083=CYLINDRICAL_SURFACE('',#11517,0.164999999999999);
#10084=CYLINDRICAL_SURFACE('',#11521,0.165);
#10085=CYLINDRICAL_SURFACE('',#11525,0.274999999999999);
#10086=CYLINDRICAL_SURFACE('',#11528,0.275);
#10087=CYLINDRICAL_SURFACE('',#11531,0.274999999999999);
#10088=CYLINDRICAL_SURFACE('',#11534,0.275);
#10089=CYLINDRICAL_SURFACE('',#11537,0.164999999999999);
#10090=CYLINDRICAL_SURFACE('',#11541,0.164999999999999);
#10091=CYLINDRICAL_SURFACE('',#11545,0.164999999999999);
#10092=CYLINDRICAL_SURFACE('',#11549,0.164999999999999);
#10093=CYLINDRICAL_SURFACE('',#11553,0.165);
#10094=CYLINDRICAL_SURFACE('',#11557,0.165);
#10095=CYLINDRICAL_SURFACE('',#11561,0.165);
#10096=CYLINDRICAL_SURFACE('',#11565,0.165);
#10097=CYLINDRICAL_SURFACE('',#11602,0.165);
#10098=CYLINDRICAL_SURFACE('',#11605,0.165);
#10099=CYLINDRICAL_SURFACE('',#11608,0.165);
#10100=CYLINDRICAL_SURFACE('',#11611,0.165);
#10101=CYLINDRICAL_SURFACE('',#11614,1.5);
#10102=CYLINDRICAL_SURFACE('',#11617,0.225);
#10103=CYLINDRICAL_SURFACE('',#11620,0.225);
#10104=CYLINDRICAL_SURFACE('',#11623,0.225);
#10105=CYLINDRICAL_SURFACE('',#11626,0.225);
#10106=CYLINDRICAL_SURFACE('',#11640,1.1);
#10107=CYLINDRICAL_SURFACE('',#11643,1.49);
#10108=CYLINDRICAL_SURFACE('',#11649,0.225);
#10109=CYLINDRICAL_SURFACE('',#11652,0.225);
#10110=CYLINDRICAL_SURFACE('',#11655,0.225);
#10111=CYLINDRICAL_SURFACE('',#11658,0.225);
#10112=CYLINDRICAL_SURFACE('',#11667,2.1);
#10113=CYLINDRICAL_SURFACE('',#11669,2.1);
#10114=CYLINDRICAL_SURFACE('',#11671,2.1);
#10115=CYLINDRICAL_SURFACE('',#11673,2.1);
#10116=CYLINDRICAL_SURFACE('',#11675,1.49);
#10117=CYLINDRICAL_SURFACE('',#11680,1.1);
#10118=CYLINDRICAL_SURFACE('',#11683,0.225);
#10119=CYLINDRICAL_SURFACE('',#11686,0.225);
#10120=CYLINDRICAL_SURFACE('',#11689,0.225);
#10121=CYLINDRICAL_SURFACE('',#11692,0.225);
#10122=CYLINDRICAL_SURFACE('',#11701,2.1);
#10123=CYLINDRICAL_SURFACE('',#11703,2.1);
#10124=CYLINDRICAL_SURFACE('',#11705,2.1);
#10125=CYLINDRICAL_SURFACE('',#11707,2.1);
#10126=CYLINDRICAL_SURFACE('',#11709,1.49);
#10127=CYLINDRICAL_SURFACE('',#11713,1.1);
#10128=CYLINDRICAL_SURFACE('',#11717,0.164999999999999);
#10129=CYLINDRICAL_SURFACE('',#11720,0.164999999999999);
#10130=CYLINDRICAL_SURFACE('',#11723,0.164999999999999);
#10131=CYLINDRICAL_SURFACE('',#11726,0.164999999999999);
#10132=CYLINDRICAL_SURFACE('',#11729,1.5);
#10133=CYLINDRICAL_SURFACE('',#11732,0.225000000000001);
#10134=CYLINDRICAL_SURFACE('',#11735,0.225000000000001);
#10135=CYLINDRICAL_SURFACE('',#11738,0.225000000000001);
#10136=CYLINDRICAL_SURFACE('',#11741,0.225000000000001);
#10137=CYLINDRICAL_SURFACE('',#11755,1.1);
#10138=CYLINDRICAL_SURFACE('',#11758,1.49);
#10139=CYLINDRICAL_SURFACE('',#11764,0.225000000000001);
#10140=CYLINDRICAL_SURFACE('',#11767,0.225000000000001);
#10141=CYLINDRICAL_SURFACE('',#11770,0.225000000000001);
#10142=CYLINDRICAL_SURFACE('',#11773,0.225000000000001);
#10143=CYLINDRICAL_SURFACE('',#11782,2.1);
#10144=CYLINDRICAL_SURFACE('',#11784,2.1);
#10145=CYLINDRICAL_SURFACE('',#11786,2.1);
#10146=CYLINDRICAL_SURFACE('',#11788,2.1);
#10147=CYLINDRICAL_SURFACE('',#11790,1.49);
#10148=CYLINDRICAL_SURFACE('',#11795,1.1);
#10149=CYLINDRICAL_SURFACE('',#11798,0.225000000000001);
#10150=CYLINDRICAL_SURFACE('',#11801,0.225000000000001);
#10151=CYLINDRICAL_SURFACE('',#11804,0.225000000000001);
#10152=CYLINDRICAL_SURFACE('',#11807,0.225000000000001);
#10153=CYLINDRICAL_SURFACE('',#11816,2.1);
#10154=CYLINDRICAL_SURFACE('',#11818,2.1);
#10155=CYLINDRICAL_SURFACE('',#11820,2.1);
#10156=CYLINDRICAL_SURFACE('',#11822,2.1);
#10157=CYLINDRICAL_SURFACE('',#11824,1.49);
#10158=CYLINDRICAL_SURFACE('',#11828,1.1);
#10159=CYLINDRICAL_SURFACE('',#11839,0.636619772367581);
#10160=CYLINDRICAL_SURFACE('',#11841,0.636619772367581);
#10161=CYLINDRICAL_SURFACE('',#11843,0.736619772367582);
#10162=CYLINDRICAL_SURFACE('',#11847,0.736619772367581);
#10163=CYLINDRICAL_SURFACE('',#11851,0.4);
#10164=CYLINDRICAL_SURFACE('',#11854,0.4);
#10165=CYLINDRICAL_SURFACE('',#11859,0.4);
#10166=CYLINDRICAL_SURFACE('',#11862,0.4);
#10167=CYLINDRICAL_SURFACE('',#11871,0.225);
#10168=CYLINDRICAL_SURFACE('',#11873,0.225);
#10169=CYLINDRICAL_SURFACE('',#11884,0.399999999999999);
#10170=CYLINDRICAL_SURFACE('',#11887,0.399999999999999);
#10171=CYLINDRICAL_SURFACE('',#11892,0.399999999999999);
#10172=CYLINDRICAL_SURFACE('',#11895,0.399999999999999);
#10173=CYLINDRICAL_SURFACE('',#11904,0.225000000000001);
#10174=CYLINDRICAL_SURFACE('',#11906,0.225000000000001);
#10175=CYLINDRICAL_SURFACE('',#11924,0.976185);
#10176=CYLINDRICAL_SURFACE('',#11926,0.5);
#10177=CYLINDRICAL_SURFACE('',#11932,0.976185);
#10178=CYLINDRICAL_SURFACE('',#11944,1.023815);
#10179=CYLINDRICAL_SURFACE('',#11951,1.5);
#10180=CYLINDRICAL_SURFACE('',#11956,1.023815);
#10181=CYLINDRICAL_SURFACE('',#11978,1.019052);
#10182=CYLINDRICAL_SURFACE('',#12018,0.980948);
#10183=CYLINDRICAL_SURFACE('',#12032,1.013815);
#10184=CYLINDRICAL_SURFACE('',#12036,0.991185);
#10185=CYLINDRICAL_SURFACE('',#12040,1.013815);
#10186=CYLINDRICAL_SURFACE('',#12044,0.991185);
#10187=CYLINDRICAL_SURFACE('',#12087,0.21);
#10188=CYLINDRICAL_SURFACE('',#12112,0.2117);
#10189=CYLINDRICAL_SURFACE('',#12136,0.425);
#10190=CYLINDRICAL_SURFACE('',#12144,0.24505);
#10191=CYLINDRICAL_SURFACE('',#12146,0.375);
#10192=CYLINDRICAL_SURFACE('',#12151,0.375);
#10193=CYLINDRICAL_SURFACE('',#12156,0.375);
#10194=CYLINDRICAL_SURFACE('',#12161,0.375);
#10195=CYLINDRICAL_SURFACE('',#12166,0.225);
#10196=CYLINDRICAL_SURFACE('',#12168,0.225);
#10197=CYLINDRICAL_SURFACE('',#12170,0.225);
#10198=CYLINDRICAL_SURFACE('',#12172,0.225000000000001);
#10199=CYLINDRICAL_SURFACE('',#12190,0.165);
#10200=CYLINDRICAL_SURFACE('',#12200,0.7);
#10201=CYLINDRICAL_SURFACE('',#12201,0.5);
#10202=CYLINDRICAL_SURFACE('',#12203,0.4);
#10203=CYLINDRICAL_SURFACE('',#12207,0.5);
#10204=CYLINDRICAL_SURFACE('',#12212,0.505);
#10205=CYLINDRICAL_SURFACE('',#12217,0.405);
#10206=CYLINDRICAL_SURFACE('',#12219,0.7);
#10207=CYLINDRICAL_SURFACE('',#12225,0.505);
#10208=CYLINDRICAL_SURFACE('',#12228,0.7);
#10209=CYLINDRICAL_SURFACE('',#12234,0.15);
#10210=CYLINDRICAL_SURFACE('',#12240,0.15);
#10211=CYLINDRICAL_SURFACE('',#12246,0.225);
#10212=CYLINDRICAL_SURFACE('',#12249,0.6);
#10213=CYLINDRICAL_SURFACE('',#12256,0.164999999999999);
#10214=CYLINDRICAL_SURFACE('',#12266,0.700000000000003);
#10215=CYLINDRICAL_SURFACE('',#12267,0.5);
#10216=CYLINDRICAL_SURFACE('',#12269,0.399999999999999);
#10217=CYLINDRICAL_SURFACE('',#12273,0.5);
#10218=CYLINDRICAL_SURFACE('',#12278,0.505000000000003);
#10219=CYLINDRICAL_SURFACE('',#12283,0.405000000000001);
#10220=CYLINDRICAL_SURFACE('',#12285,0.700000000000003);
#10221=CYLINDRICAL_SURFACE('',#12291,0.505000000000003);
#10222=CYLINDRICAL_SURFACE('',#12294,0.700000000000003);
#10223=CYLINDRICAL_SURFACE('',#12300,0.149999999999999);
#10224=CYLINDRICAL_SURFACE('',#12306,0.149999999999999);
#10225=CYLINDRICAL_SURFACE('',#12312,0.225000000000001);
#10226=CYLINDRICAL_SURFACE('',#12315,0.600000000000001);
#10227=CYLINDRICAL_SURFACE('',#12321,0.125);
#10228=CYLINDRICAL_SURFACE('',#12322,0.125);
#10229=CYLINDRICAL_SURFACE('',#12323,0.65);
#10230=CYLINDRICAL_SURFACE('',#12326,0.125);
#10231=CYLINDRICAL_SURFACE('',#12327,0.125);
#10232=CYLINDRICAL_SURFACE('',#12328,0.4);
#10233=CYLINDRICAL_SURFACE('',#12374,0.8);
#10234=CYLINDRICAL_SURFACE('',#12419,0.8);
#10235=CYLINDRICAL_SURFACE('',#12422,0.0555);
#10236=CYLINDRICAL_SURFACE('',#12423,0.611219772367581);
#10237=CYLINDRICAL_SURFACE('',#12424,0.0555);
#10238=CYLINDRICAL_SURFACE('',#12425,0.611219772367581);
#10239=CYLINDRICAL_SURFACE('',#12426,0.0555);
#10240=CYLINDRICAL_SURFACE('',#12427,0.611219772367581);
#10241=CYLINDRICAL_SURFACE('',#12428,0.0555);
#10242=CYLINDRICAL_SURFACE('',#12429,0.611219772367581);
#10243=CYLINDRICAL_SURFACE('',#12430,0.0555);
#10244=CYLINDRICAL_SURFACE('',#12431,0.611219772367581);
#10245=CYLINDRICAL_SURFACE('',#12432,0.0555);
#10246=CYLINDRICAL_SURFACE('',#12433,0.611219772367581);
#10247=CYLINDRICAL_SURFACE('',#12434,0.0555);
#10248=CYLINDRICAL_SURFACE('',#12435,0.611219772367581);
#10249=CYLINDRICAL_SURFACE('',#12436,0.0555);
#10250=CYLINDRICAL_SURFACE('',#12437,0.611219772367581);
#10251=CYLINDRICAL_SURFACE('',#12438,0.0555);
#10252=CYLINDRICAL_SURFACE('',#12439,0.611219772367581);
#10253=CYLINDRICAL_SURFACE('',#12440,0.0555);
#10254=CYLINDRICAL_SURFACE('',#12441,0.611219772367581);
#10255=CYLINDRICAL_SURFACE('',#12442,0.0555);
#10256=CYLINDRICAL_SURFACE('',#12443,0.611219772367581);
#10257=CYLINDRICAL_SURFACE('',#12444,0.0555);
#10258=CYLINDRICAL_SURFACE('',#12445,0.611219772367581);
#10259=CYLINDRICAL_SURFACE('',#12446,0.0555);
#10260=CYLINDRICAL_SURFACE('',#12447,0.611219772367581);
#10261=CYLINDRICAL_SURFACE('',#12448,0.0555);
#10262=CYLINDRICAL_SURFACE('',#12449,0.611219772367581);
#10263=CYLINDRICAL_SURFACE('',#12450,0.0555);
#10264=CYLINDRICAL_SURFACE('',#12451,0.611219772367581);
#10265=CYLINDRICAL_SURFACE('',#12452,0.0555);
#10266=CYLINDRICAL_SURFACE('',#12453,0.611219772367581);
#10267=CYLINDRICAL_SURFACE('',#12454,0.0555);
#10268=CYLINDRICAL_SURFACE('',#12455,0.611219772367581);
#10269=CYLINDRICAL_SURFACE('',#12456,0.0555);
#10270=CYLINDRICAL_SURFACE('',#12457,0.611219772367581);
#10271=CYLINDRICAL_SURFACE('',#12458,0.0555);
#10272=CYLINDRICAL_SURFACE('',#12459,0.611219772367581);
#10273=CYLINDRICAL_SURFACE('',#12460,0.0555);
#10274=CYLINDRICAL_SURFACE('',#12461,0.611219772367581);
#10275=CYLINDRICAL_SURFACE('',#12464,0.4);
#10276=CYLINDRICAL_SURFACE('',#12469,0.399999999999999);
#10277=CYLINDRICAL_SURFACE('',#12474,0.225);
#10278=CYLINDRICAL_SURFACE('',#12476,0.225000000000001);
#10279=CYLINDRICAL_SURFACE('',#12478,0.274999999999999);
#10280=CYLINDRICAL_SURFACE('',#12481,0.275);
#10281=CYLINDRICAL_SURFACE('',#12484,0.275);
#10282=CYLINDRICAL_SURFACE('',#12487,0.274999999999999);
#10283=CYLINDRICAL_SURFACE('',#12497,0.164999999999999);
#10284=CYLINDRICAL_SURFACE('',#12501,0.164999999999999);
#10285=CYLINDRICAL_SURFACE('',#12507,0.6);
#10286=CYLINDRICAL_SURFACE('',#12509,0.600000000000001);
#10287=CYLINDRICAL_SURFACE('',#12515,0.164999999999999);
#10288=CYLINDRICAL_SURFACE('',#12519,0.164999999999999);
#10289=CYLINDRICAL_SURFACE('',#12540,0.21);
#10290=CYLINDRICAL_SURFACE('',#12546,0.21);
#10291=CYLINDRICAL_SURFACE('',#12552,0.21);
#10292=CYLINDRICAL_SURFACE('',#12558,0.21);
#10293=CYLINDRICAL_SURFACE('',#12605,0.265);
#10294=CYLINDRICAL_SURFACE('',#12609,0.5);
#10295=CYLINDRICAL_SURFACE('',#12617,0.425);
#10296=CYLINDRICAL_SURFACE('',#12625,0.24505);
#10297=CYLINDRICAL_SURFACE('',#12653,0.35);
#10298=CYLINDRICAL_SURFACE('',#12661,0.1954);
#10299=CYLINDRICAL_SURFACE('',#12667,0.35);
#10300=CYLINDRICAL_SURFACE('',#12675,0.1954);
#10301=ADVANCED_FACE('',(#1250),#10077,.F.);
#10302=ADVANCED_FACE('',(#1251),#889,.T.);
#10303=ADVANCED_FACE('',(#1252),#10078,.F.);
#10304=ADVANCED_FACE('',(#1253),#890,.T.);
#10305=ADVANCED_FACE('',(#1254),#10079,.F.);
#10306=ADVANCED_FACE('',(#1255),#891,.T.);
#10307=ADVANCED_FACE('',(#1256),#10080,.F.);
#10308=ADVANCED_FACE('',(#1257),#892,.T.);
#10309=ADVANCED_FACE('',(#1258),#10081,.F.);
#10310=ADVANCED_FACE('',(#1259),#893,.T.);
#10311=ADVANCED_FACE('',(#1260),#10082,.F.);
#10312=ADVANCED_FACE('',(#1261),#894,.T.);
#10313=ADVANCED_FACE('',(#1262),#10083,.F.);
#10314=ADVANCED_FACE('',(#1263),#895,.T.);
#10315=ADVANCED_FACE('',(#1264),#10084,.F.);
#10316=ADVANCED_FACE('',(#1265),#896,.T.);
#10317=ADVANCED_FACE('',(#1266),#10085,.F.);
#10318=ADVANCED_FACE('',(#1267),#10086,.F.);
#10319=ADVANCED_FACE('',(#1268),#10087,.F.);
#10320=ADVANCED_FACE('',(#1269),#10088,.F.);
#10321=ADVANCED_FACE('',(#1270),#10089,.F.);
#10322=ADVANCED_FACE('',(#1271),#897,.T.);
#10323=ADVANCED_FACE('',(#1272),#10090,.F.);
#10324=ADVANCED_FACE('',(#1273),#898,.T.);
#10325=ADVANCED_FACE('',(#1274),#10091,.F.);
#10326=ADVANCED_FACE('',(#1275),#899,.T.);
#10327=ADVANCED_FACE('',(#1276),#10092,.F.);
#10328=ADVANCED_FACE('',(#1277),#900,.T.);
#10329=ADVANCED_FACE('',(#1278),#10093,.F.);
#10330=ADVANCED_FACE('',(#1279),#901,.T.);
#10331=ADVANCED_FACE('',(#1280),#10094,.F.);
#10332=ADVANCED_FACE('',(#1281),#902,.T.);
#10333=ADVANCED_FACE('',(#1282),#10095,.F.);
#10334=ADVANCED_FACE('',(#1283),#903,.T.);
#10335=ADVANCED_FACE('',(#1284),#10096,.F.);
#10336=ADVANCED_FACE('',(#1285),#904,.T.);
#10337=ADVANCED_FACE('',(#1286),#905,.T.);
#10338=ADVANCED_FACE('',(#1287),#906,.T.);
#10339=ADVANCED_FACE('',(#1288),#907,.T.);
#10340=ADVANCED_FACE('',(#1289),#908,.T.);
#10341=ADVANCED_FACE('',(#1290,#718,#719,#720,#721,#722,#723,#724,#725,
#726,#727,#728,#729,#730,#731,#732,#733,#734,#735,#736,#737),#909,.T.);
#10342=ADVANCED_FACE('',(#1291,#738,#739,#740,#741),#910,.F.);
#10343=ADVANCED_FACE('',(#1292),#911,.F.);
#10344=ADVANCED_FACE('',(#1293),#912,.T.);
#10345=ADVANCED_FACE('',(#1294),#913,.T.);
#10346=ADVANCED_FACE('',(#1295),#914,.F.);
#10347=ADVANCED_FACE('',(#1296),#915,.F.);
#10348=ADVANCED_FACE('',(#1297),#916,.T.);
#10349=ADVANCED_FACE('',(#1298),#917,.T.);
#10350=ADVANCED_FACE('',(#1299),#918,.T.);
#10351=ADVANCED_FACE('',(#1300),#919,.T.);
#10352=ADVANCED_FACE('',(#1301),#920,.T.);
#10353=ADVANCED_FACE('',(#1302),#921,.F.);
#10354=ADVANCED_FACE('',(#1303),#922,.F.);
#10355=ADVANCED_FACE('',(#1304),#923,.F.);
#10356=ADVANCED_FACE('',(#1305),#924,.T.);
#10357=ADVANCED_FACE('',(#1306),#925,.T.);
#10358=ADVANCED_FACE('',(#1307),#926,.F.);
#10359=ADVANCED_FACE('',(#1308),#927,.F.);
#10360=ADVANCED_FACE('',(#1309),#928,.T.);
#10361=ADVANCED_FACE('',(#1310),#929,.T.);
#10362=ADVANCED_FACE('',(#1311),#930,.T.);
#10363=ADVANCED_FACE('',(#1312),#931,.T.);
#10364=ADVANCED_FACE('',(#1313),#932,.T.);
#10365=ADVANCED_FACE('',(#1314),#933,.F.);
#10366=ADVANCED_FACE('',(#1315),#934,.F.);
#10367=ADVANCED_FACE('',(#1316),#10097,.F.);
#10368=ADVANCED_FACE('',(#1317),#10098,.F.);
#10369=ADVANCED_FACE('',(#1318),#10099,.F.);
#10370=ADVANCED_FACE('',(#1319),#10100,.F.);
#10371=ADVANCED_FACE('',(#1320),#10101,.F.);
#10372=ADVANCED_FACE('',(#1321),#10102,.F.);
#10373=ADVANCED_FACE('',(#1322),#10103,.F.);
#10374=ADVANCED_FACE('',(#1323),#10104,.F.);
#10375=ADVANCED_FACE('',(#1324),#10105,.F.);
#10376=ADVANCED_FACE('',(#1325,#742,#743),#935,.T.);
#10377=ADVANCED_FACE('',(#1326,#744,#745),#936,.T.);
#10378=ADVANCED_FACE('',(#1327),#937,.T.);
#10379=ADVANCED_FACE('',(#1328),#938,.T.);
#10380=ADVANCED_FACE('',(#1329,#746,#747,#748,#749,#750),#939,.T.);
#10381=ADVANCED_FACE('',(#1330),#940,.T.);
#10382=ADVANCED_FACE('',(#1331,#751,#752,#753,#754,#755),#941,.T.);
#10383=ADVANCED_FACE('',(#1332),#942,.T.);
#10384=ADVANCED_FACE('',(#1333),#943,.T.);
#10385=ADVANCED_FACE('',(#1334,#756,#757,#758,#759),#944,.F.);
#10386=ADVANCED_FACE('',(#1335),#10106,.F.);
#10387=ADVANCED_FACE('',(#1336),#10107,.T.);
#10388=ADVANCED_FACE('',(#1337,#760),#945,.T.);
#10389=ADVANCED_FACE('',(#1338,#761),#946,.F.);
#10390=ADVANCED_FACE('',(#1339),#10108,.F.);
#10391=ADVANCED_FACE('',(#1340),#10109,.F.);
#10392=ADVANCED_FACE('',(#1341),#10110,.F.);
#10393=ADVANCED_FACE('',(#1342),#10111,.F.);
#10394=ADVANCED_FACE('',(#1343,#762),#947,.F.);
#10395=ADVANCED_FACE('',(#1344),#10112,.T.);
#10396=ADVANCED_FACE('',(#1345),#10113,.T.);
#10397=ADVANCED_FACE('',(#1346),#10114,.T.);
#10398=ADVANCED_FACE('',(#1347),#10115,.T.);
#10399=ADVANCED_FACE('',(#1348),#10116,.T.);
#10400=ADVANCED_FACE('',(#1349,#763),#948,.T.);
#10401=ADVANCED_FACE('',(#1350),#10117,.F.);
#10402=ADVANCED_FACE('',(#1351,#764),#949,.T.);
#10403=ADVANCED_FACE('',(#1352),#10118,.F.);
#10404=ADVANCED_FACE('',(#1353),#10119,.F.);
#10405=ADVANCED_FACE('',(#1354),#10120,.F.);
#10406=ADVANCED_FACE('',(#1355),#10121,.F.);
#10407=ADVANCED_FACE('',(#1356,#765),#950,.F.);
#10408=ADVANCED_FACE('',(#1357),#10122,.T.);
#10409=ADVANCED_FACE('',(#1358),#10123,.T.);
#10410=ADVANCED_FACE('',(#1359),#10124,.T.);
#10411=ADVANCED_FACE('',(#1360),#10125,.T.);
#10412=ADVANCED_FACE('',(#1361),#10126,.T.);
#10413=ADVANCED_FACE('',(#1362,#766),#951,.F.);
#10414=ADVANCED_FACE('',(#1363),#10127,.F.);
#10415=ADVANCED_FACE('',(#1364,#767),#952,.T.);
#10416=ADVANCED_FACE('',(#1365),#10128,.F.);
#10417=ADVANCED_FACE('',(#1366),#10129,.F.);
#10418=ADVANCED_FACE('',(#1367),#10130,.F.);
#10419=ADVANCED_FACE('',(#1368),#10131,.F.);
#10420=ADVANCED_FACE('',(#1369),#10132,.F.);
#10421=ADVANCED_FACE('',(#1370),#10133,.F.);
#10422=ADVANCED_FACE('',(#1371),#10134,.F.);
#10423=ADVANCED_FACE('',(#1372),#10135,.F.);
#10424=ADVANCED_FACE('',(#1373),#10136,.F.);
#10425=ADVANCED_FACE('',(#1374,#768,#769),#953,.T.);
#10426=ADVANCED_FACE('',(#1375,#770,#771),#954,.T.);
#10427=ADVANCED_FACE('',(#1376),#955,.T.);
#10428=ADVANCED_FACE('',(#1377),#956,.T.);
#10429=ADVANCED_FACE('',(#1378,#772,#773,#774,#775,#776),#957,.T.);
#10430=ADVANCED_FACE('',(#1379),#958,.T.);
#10431=ADVANCED_FACE('',(#1380,#777,#778,#779,#780,#781),#959,.T.);
#10432=ADVANCED_FACE('',(#1381),#960,.T.);
#10433=ADVANCED_FACE('',(#1382),#961,.T.);
#10434=ADVANCED_FACE('',(#1383,#782,#783,#784,#785),#962,.F.);
#10435=ADVANCED_FACE('',(#1384),#10137,.F.);
#10436=ADVANCED_FACE('',(#1385),#10138,.T.);
#10437=ADVANCED_FACE('',(#1386,#786),#963,.T.);
#10438=ADVANCED_FACE('',(#1387,#787),#964,.F.);
#10439=ADVANCED_FACE('',(#1388),#10139,.F.);
#10440=ADVANCED_FACE('',(#1389),#10140,.F.);
#10441=ADVANCED_FACE('',(#1390),#10141,.F.);
#10442=ADVANCED_FACE('',(#1391),#10142,.F.);
#10443=ADVANCED_FACE('',(#1392,#788),#965,.F.);
#10444=ADVANCED_FACE('',(#1393),#10143,.T.);
#10445=ADVANCED_FACE('',(#1394),#10144,.T.);
#10446=ADVANCED_FACE('',(#1395),#10145,.T.);
#10447=ADVANCED_FACE('',(#1396),#10146,.T.);
#10448=ADVANCED_FACE('',(#1397),#10147,.T.);
#10449=ADVANCED_FACE('',(#1398,#789),#966,.T.);
#10450=ADVANCED_FACE('',(#1399),#10148,.F.);
#10451=ADVANCED_FACE('',(#1400,#790),#967,.T.);
#10452=ADVANCED_FACE('',(#1401),#10149,.F.);
#10453=ADVANCED_FACE('',(#1402),#10150,.F.);
#10454=ADVANCED_FACE('',(#1403),#10151,.F.);
#10455=ADVANCED_FACE('',(#1404),#10152,.F.);
#10456=ADVANCED_FACE('',(#1405,#791),#968,.F.);
#10457=ADVANCED_FACE('',(#1406),#10153,.T.);
#10458=ADVANCED_FACE('',(#1407),#10154,.T.);
#10459=ADVANCED_FACE('',(#1408),#10155,.T.);
#10460=ADVANCED_FACE('',(#1409),#10156,.T.);
#10461=ADVANCED_FACE('',(#1410),#10157,.T.);
#10462=ADVANCED_FACE('',(#1411,#792),#969,.F.);
#10463=ADVANCED_FACE('',(#1412),#10158,.F.);
#10464=ADVANCED_FACE('',(#1413,#793),#970,.T.);
#10465=ADVANCED_FACE('',(#1414),#971,.F.);
#10466=ADVANCED_FACE('',(#1415),#972,.F.);
#10467=ADVANCED_FACE('',(#1416,#794),#973,.F.);
#10468=ADVANCED_FACE('',(#1417),#10159,.F.);
#10469=ADVANCED_FACE('',(#1418),#10160,.F.);
#10470=ADVANCED_FACE('',(#1419),#10161,.T.);
#10471=ADVANCED_FACE('',(#1420),#974,.T.);
#10472=ADVANCED_FACE('',(#1421),#975,.T.);
#10473=ADVANCED_FACE('',(#1422),#10162,.T.);
#10474=ADVANCED_FACE('',(#1423,#795),#976,.T.);
#10475=ADVANCED_FACE('',(#1424),#10163,.F.);
#10476=ADVANCED_FACE('',(#1425),#10164,.F.);
#10477=ADVANCED_FACE('',(#1426,#796),#977,.T.);
#10478=ADVANCED_FACE('',(#1427),#10165,.F.);
#10479=ADVANCED_FACE('',(#1428),#10166,.F.);
#10480=ADVANCED_FACE('',(#1429,#797),#978,.T.);
#10481=ADVANCED_FACE('',(#1430),#979,.T.);
#10482=ADVANCED_FACE('',(#1431),#980,.T.);
#10483=ADVANCED_FACE('',(#1432),#981,.T.);
#10484=ADVANCED_FACE('',(#1433),#982,.T.);
#10485=ADVANCED_FACE('',(#1434),#10167,.F.);
#10486=ADVANCED_FACE('',(#1435),#10168,.F.);
#10487=ADVANCED_FACE('',(#1436),#983,.F.);
#10488=ADVANCED_FACE('',(#1437),#984,.F.);
#10489=ADVANCED_FACE('',(#1438),#985,.F.);
#10490=ADVANCED_FACE('',(#1439),#986,.T.);
#10491=ADVANCED_FACE('',(#1440,#798),#987,.F.);
#10492=ADVANCED_FACE('',(#1441,#799),#988,.F.);
#10493=ADVANCED_FACE('',(#1442),#989,.T.);
#10494=ADVANCED_FACE('',(#1443),#990,.T.);
#10495=ADVANCED_FACE('',(#1444),#10169,.F.);
#10496=ADVANCED_FACE('',(#1445),#10170,.F.);
#10497=ADVANCED_FACE('',(#1446,#800),#991,.T.);
#10498=ADVANCED_FACE('',(#1447),#10171,.F.);
#10499=ADVANCED_FACE('',(#1448),#10172,.F.);
#10500=ADVANCED_FACE('',(#1449,#801),#992,.T.);
#10501=ADVANCED_FACE('',(#1450),#993,.T.);
#10502=ADVANCED_FACE('',(#1451),#994,.T.);
#10503=ADVANCED_FACE('',(#1452),#995,.T.);
#10504=ADVANCED_FACE('',(#1453),#996,.T.);
#10505=ADVANCED_FACE('',(#1454),#10173,.F.);
#10506=ADVANCED_FACE('',(#1455),#10174,.F.);
#10507=ADVANCED_FACE('',(#1456),#997,.F.);
#10508=ADVANCED_FACE('',(#1457),#998,.F.);
#10509=ADVANCED_FACE('',(#1458),#999,.F.);
#10510=ADVANCED_FACE('',(#1459),#1000,.T.);
#10511=ADVANCED_FACE('',(#1460,#802),#1001,.F.);
#10512=ADVANCED_FACE('',(#1461,#803),#1002,.F.);
#10513=ADVANCED_FACE('',(#1462),#1003,.T.);
#10514=ADVANCED_FACE('',(#1463),#1004,.T.);
#10515=ADVANCED_FACE('',(#1464),#516,.F.);
#10516=ADVANCED_FACE('',(#1465),#10175,.T.);
#10517=ADVANCED_FACE('',(#1466),#10176,.F.);
#10518=ADVANCED_FACE('',(#1467),#497,.F.);
#10519=ADVANCED_FACE('',(#1468,#804),#1005,.T.);
#10520=ADVANCED_FACE('',(#1469),#10177,.T.);
#10521=ADVANCED_FACE('',(#1470,#805),#1006,.T.);
#10522=ADVANCED_FACE('',(#1471),#498,.F.);
#10523=ADVANCED_FACE('',(#1472),#517,.F.);
#10524=ADVANCED_FACE('',(#1473),#10178,.F.);
#10525=ADVANCED_FACE('',(#1474,#806),#1007,.T.);
#10526=ADVANCED_FACE('',(#1475),#499,.T.);
#10527=ADVANCED_FACE('',(#1476),#10179,.T.);
#10528=ADVANCED_FACE('',(#1477),#500,.T.);
#10529=ADVANCED_FACE('',(#1478,#807),#1008,.T.);
#10530=ADVANCED_FACE('',(#1479),#10180,.F.);
#10531=ADVANCED_FACE('',(#1480),#481,.T.);
#10532=ADVANCED_FACE('',(#1481),#482,.T.);
#10533=ADVANCED_FACE('',(#1482),#483,.T.);
#10534=ADVANCED_FACE('',(#1483),#484,.T.);
#10535=ADVANCED_FACE('',(#1484),#485,.T.);
#10536=ADVANCED_FACE('',(#1485),#486,.T.);
#10537=ADVANCED_FACE('',(#1486),#487,.T.);
#10538=ADVANCED_FACE('',(#1487),#488,.T.);
#10539=ADVANCED_FACE('',(#1488),#489,.F.);
#10540=ADVANCED_FACE('',(#1489),#10181,.T.);
#10541=ADVANCED_FACE('',(#1490),#1009,.T.);
#10542=ADVANCED_FACE('',(#1491),#490,.F.);
#10543=ADVANCED_FACE('',(#1492),#1010,.T.);
#10544=ADVANCED_FACE('',(#1493),#491,.F.);
#10545=ADVANCED_FACE('',(#1494),#1011,.T.);
#10546=ADVANCED_FACE('',(#1495),#492,.F.);
#10547=ADVANCED_FACE('',(#1496),#1012,.T.);
#10548=ADVANCED_FACE('',(#1497),#493,.F.);
#10549=ADVANCED_FACE('',(#1498),#1013,.T.);
#10550=ADVANCED_FACE('',(#1499),#494,.F.);
#10551=ADVANCED_FACE('',(#1500),#1014,.T.);
#10552=ADVANCED_FACE('',(#1501),#495,.F.);
#10553=ADVANCED_FACE('',(#1502),#10182,.F.);
#10554=ADVANCED_FACE('',(#1503),#1015,.T.);
#10555=ADVANCED_FACE('',(#1504),#496,.F.);
#10556=ADVANCED_FACE('',(#1505,#808),#1016,.T.);
#10557=ADVANCED_FACE('',(#1506),#1017,.T.);
#10558=ADVANCED_FACE('',(#1507,#809),#1018,.T.);
#10559=ADVANCED_FACE('',(#1508),#10183,.T.);
#10560=ADVANCED_FACE('',(#1509,#810),#1019,.T.);
#10561=ADVANCED_FACE('',(#1510),#10184,.F.);
#10562=ADVANCED_FACE('',(#1511,#811),#1020,.T.);
#10563=ADVANCED_FACE('',(#1512),#10185,.T.);
#10564=ADVANCED_FACE('',(#1513,#812),#1021,.T.);
#10565=ADVANCED_FACE('',(#1514),#10186,.F.);
#10566=ADVANCED_FACE('',(#1515),#1022,.F.);
#10567=ADVANCED_FACE('',(#1516),#1023,.F.);
#10568=ADVANCED_FACE('',(#1517),#1024,.F.);
#10569=ADVANCED_FACE('',(#1518),#1025,.F.);
#10570=ADVANCED_FACE('',(#1519),#1026,.F.);
#10571=ADVANCED_FACE('',(#1520),#1027,.F.);
#10572=ADVANCED_FACE('',(#1521),#1028,.F.);
#10573=ADVANCED_FACE('',(#1522),#1029,.F.);
#10574=ADVANCED_FACE('',(#1523),#1030,.F.);
#10575=ADVANCED_FACE('',(#1524),#1031,.F.);
#10576=ADVANCED_FACE('',(#1525),#1032,.F.);
#10577=ADVANCED_FACE('',(#1526),#1033,.F.);
#10578=ADVANCED_FACE('',(#1527),#1034,.F.);
#10579=ADVANCED_FACE('',(#1528),#1035,.F.);
#10580=ADVANCED_FACE('',(#1529),#1036,.F.);
#10581=ADVANCED_FACE('',(#1530),#1037,.F.);
#10582=ADVANCED_FACE('',(#1531),#1038,.F.);
#10583=ADVANCED_FACE('',(#1532),#1039,.F.);
#10584=ADVANCED_FACE('',(#1533),#1040,.F.);
#10585=ADVANCED_FACE('',(#1534),#1041,.F.);
#10586=ADVANCED_FACE('',(#1535),#1042,.F.);
#10587=ADVANCED_FACE('',(#1536),#1043,.F.);
#10588=ADVANCED_FACE('',(#1537),#1044,.F.);
#10589=ADVANCED_FACE('',(#1538),#1045,.F.);
#10590=ADVANCED_FACE('',(#1539),#1046,.F.);
#10591=ADVANCED_FACE('',(#1540),#1047,.F.);
#10592=ADVANCED_FACE('',(#1541),#1048,.F.);
#10593=ADVANCED_FACE('',(#1542),#1049,.F.);
#10594=ADVANCED_FACE('',(#1543),#1050,.F.);
#10595=ADVANCED_FACE('',(#1544),#1051,.F.);
#10596=ADVANCED_FACE('',(#1545),#1052,.F.);
#10597=ADVANCED_FACE('',(#1546),#1053,.F.);
#10598=ADVANCED_FACE('',(#1547),#1054,.F.);
#10599=ADVANCED_FACE('',(#1548),#1055,.F.);
#10600=ADVANCED_FACE('',(#1549),#1056,.F.);
#10601=ADVANCED_FACE('',(#1550),#1057,.F.);
#10602=ADVANCED_FACE('',(#1551),#10187,.F.);
#10603=ADVANCED_FACE('',(#1552),#1058,.T.);
#10604=ADVANCED_FACE('',(#1553),#1059,.T.);
#10605=ADVANCED_FACE('',(#1554),#1060,.T.);
#10606=ADVANCED_FACE('',(#1555),#1061,.T.);
#10607=ADVANCED_FACE('',(#1556),#1062,.T.);
#10608=ADVANCED_FACE('',(#1557),#1063,.T.);
#10609=ADVANCED_FACE('',(#1558),#1064,.T.);
#10610=ADVANCED_FACE('',(#1559),#1065,.T.);
#10611=ADVANCED_FACE('',(#1560,#813),#1066,.T.);
#10612=ADVANCED_FACE('',(#1561,#814),#1067,.F.);
#10613=ADVANCED_FACE('',(#1562),#1068,.F.);
#10614=ADVANCED_FACE('',(#1563),#1069,.T.);
#10615=ADVANCED_FACE('',(#1564,#815),#1070,.T.);
#10616=ADVANCED_FACE('',(#1565),#1071,.T.);
#10617=ADVANCED_FACE('',(#1566),#1072,.T.);
#10618=ADVANCED_FACE('',(#1567),#1073,.F.);
#10619=ADVANCED_FACE('',(#1568),#1074,.T.);
#10620=ADVANCED_FACE('',(#1569),#1075,.T.);
#10621=ADVANCED_FACE('',(#1570),#1076,.T.);
#10622=ADVANCED_FACE('',(#1571),#10188,.F.);
#10623=ADVANCED_FACE('',(#1572),#1077,.F.);
#10624=ADVANCED_FACE('',(#1573),#1078,.F.);
#10625=ADVANCED_FACE('',(#1574),#1079,.T.);
#10626=ADVANCED_FACE('',(#1575),#1080,.T.);
#10627=ADVANCED_FACE('',(#1576),#1081,.F.);
#10628=ADVANCED_FACE('',(#1577),#1082,.F.);
#10629=ADVANCED_FACE('',(#1578),#1083,.F.);
#10630=ADVANCED_FACE('',(#1579),#1084,.F.);
#10631=ADVANCED_FACE('',(#1580),#1085,.F.);
#10632=ADVANCED_FACE('',(#1581),#1086,.F.);
#10633=ADVANCED_FACE('',(#1582),#1087,.F.);
#10634=ADVANCED_FACE('',(#1583),#1088,.F.);
#10635=ADVANCED_FACE('',(#1584),#1089,.F.);
#10636=ADVANCED_FACE('',(#1585),#1090,.T.);
#10637=ADVANCED_FACE('',(#1586),#501,.T.);
#10638=ADVANCED_FACE('',(#1587),#10189,.T.);
#10639=ADVANCED_FACE('',(#1588),#502,.T.);
#10640=ADVANCED_FACE('',(#1589,#816),#1091,.T.);
#10641=ADVANCED_FACE('',(#1590),#503,.T.);
#10642=ADVANCED_FACE('',(#1591),#10190,.T.);
#10643=ADVANCED_FACE('',(#1592),#10191,.F.);
#10644=ADVANCED_FACE('',(#1593,#817),#1092,.T.);
#10645=ADVANCED_FACE('',(#1594),#10192,.F.);
#10646=ADVANCED_FACE('',(#1595,#818),#1093,.T.);
#10647=ADVANCED_FACE('',(#1596),#10193,.F.);
#10648=ADVANCED_FACE('',(#1597,#819),#1094,.T.);
#10649=ADVANCED_FACE('',(#1598),#10194,.F.);
#10650=ADVANCED_FACE('',(#1599,#820),#1095,.T.);
#10651=ADVANCED_FACE('',(#1600),#10195,.F.);
#10652=ADVANCED_FACE('',(#1601),#10196,.F.);
#10653=ADVANCED_FACE('',(#1602),#10197,.F.);
#10654=ADVANCED_FACE('',(#1603),#10198,.F.);
#10655=ADVANCED_FACE('',(#1604),#1096,.T.);
#10656=ADVANCED_FACE('',(#1605),#1097,.T.);
#10657=ADVANCED_FACE('',(#1606),#1098,.T.);
#10658=ADVANCED_FACE('',(#1607),#1099,.T.);
#10659=ADVANCED_FACE('',(#1608,#821,#822,#823,#824),#1100,.T.);
#10660=ADVANCED_FACE('',(#1609),#1101,.T.);
#10661=ADVANCED_FACE('',(#1610),#1102,.T.);
#10662=ADVANCED_FACE('',(#1611),#1103,.T.);
#10663=ADVANCED_FACE('',(#1612),#1104,.T.);
#10664=ADVANCED_FACE('',(#1613),#1105,.T.);
#10665=ADVANCED_FACE('',(#1614,#825,#826,#827,#828),#1106,.T.);
#10666=ADVANCED_FACE('',(#1615),#1107,.T.);
#10667=ADVANCED_FACE('',(#1616),#1108,.T.);
#10668=ADVANCED_FACE('',(#1617),#1109,.F.);
#10669=ADVANCED_FACE('',(#1618),#10199,.F.);
#10670=ADVANCED_FACE('',(#1619),#1110,.F.);
#10671=ADVANCED_FACE('',(#1620,#829),#1111,.T.);
#10672=ADVANCED_FACE('',(#1621,#830),#1112,.F.);
#10673=ADVANCED_FACE('',(#1622),#10200,.T.);
#10674=ADVANCED_FACE('',(#1623),#10201,.T.);
#10675=ADVANCED_FACE('',(#1624),#10202,.T.);
#10676=ADVANCED_FACE('',(#1625,#831),#1113,.F.);
#10677=ADVANCED_FACE('',(#1626),#10203,.T.);
#10678=ADVANCED_FACE('',(#1627),#1114,.T.);
#10679=ADVANCED_FACE('',(#1628,#832),#1115,.F.);
#10680=ADVANCED_FACE('',(#1629),#10204,.F.);
#10681=ADVANCED_FACE('',(#1630,#833),#1116,.T.);
#10682=ADVANCED_FACE('',(#1631),#10205,.F.);
#10683=ADVANCED_FACE('',(#1632),#10206,.T.);
#10684=ADVANCED_FACE('',(#1633,#834),#1117,.T.);
#10685=ADVANCED_FACE('',(#1634,#835),#1118,.F.);
#10686=ADVANCED_FACE('',(#1635),#10207,.F.);
#10687=ADVANCED_FACE('',(#1636),#10208,.T.);
#10688=ADVANCED_FACE('',(#1637,#836),#1119,.T.);
#10689=ADVANCED_FACE('',(#1638,#837),#1120,.F.);
#10690=ADVANCED_FACE('',(#1639),#10209,.T.);
#10691=ADVANCED_FACE('',(#1640),#1121,.T.);
#10692=ADVANCED_FACE('',(#1641),#1122,.F.);
#10693=ADVANCED_FACE('',(#1642),#10210,.T.);
#10694=ADVANCED_FACE('',(#1643),#1123,.T.);
#10695=ADVANCED_FACE('',(#1644),#1124,.F.);
#10696=ADVANCED_FACE('',(#1645),#10211,.F.);
#10697=ADVANCED_FACE('',(#1646),#10212,.T.);
#10698=ADVANCED_FACE('',(#1647,#838),#1125,.T.);
#10699=ADVANCED_FACE('',(#1648,#839),#1126,.F.);
#10700=ADVANCED_FACE('',(#1649),#10213,.F.);
#10701=ADVANCED_FACE('',(#1650),#1127,.F.);
#10702=ADVANCED_FACE('',(#1651,#840),#1128,.T.);
#10703=ADVANCED_FACE('',(#1652,#841),#1129,.F.);
#10704=ADVANCED_FACE('',(#1653),#10214,.T.);
#10705=ADVANCED_FACE('',(#1654),#10215,.T.);
#10706=ADVANCED_FACE('',(#1655),#10216,.T.);
#10707=ADVANCED_FACE('',(#1656,#842),#1130,.F.);
#10708=ADVANCED_FACE('',(#1657),#10217,.T.);
#10709=ADVANCED_FACE('',(#1658),#1131,.T.);
#10710=ADVANCED_FACE('',(#1659,#843),#1132,.F.);
#10711=ADVANCED_FACE('',(#1660),#10218,.F.);
#10712=ADVANCED_FACE('',(#1661,#844),#1133,.T.);
#10713=ADVANCED_FACE('',(#1662),#10219,.F.);
#10714=ADVANCED_FACE('',(#1663),#10220,.T.);
#10715=ADVANCED_FACE('',(#1664,#845),#1134,.T.);
#10716=ADVANCED_FACE('',(#1665,#846),#1135,.F.);
#10717=ADVANCED_FACE('',(#1666),#10221,.F.);
#10718=ADVANCED_FACE('',(#1667),#10222,.T.);
#10719=ADVANCED_FACE('',(#1668,#847),#1136,.T.);
#10720=ADVANCED_FACE('',(#1669,#848),#1137,.F.);
#10721=ADVANCED_FACE('',(#1670),#10223,.T.);
#10722=ADVANCED_FACE('',(#1671),#1138,.T.);
#10723=ADVANCED_FACE('',(#1672),#1139,.F.);
#10724=ADVANCED_FACE('',(#1673),#10224,.T.);
#10725=ADVANCED_FACE('',(#1674),#1140,.T.);
#10726=ADVANCED_FACE('',(#1675),#1141,.F.);
#10727=ADVANCED_FACE('',(#1676),#10225,.F.);
#10728=ADVANCED_FACE('',(#1677),#10226,.T.);
#10729=ADVANCED_FACE('',(#1678,#849),#1142,.T.);
#10730=ADVANCED_FACE('',(#1679,#850),#1143,.F.);
#10731=ADVANCED_FACE('',(#1680),#10227,.F.);
#10732=ADVANCED_FACE('',(#1681),#10228,.F.);
#10733=ADVANCED_FACE('',(#1682,#851,#852,#853),#10229,.T.);
#10734=ADVANCED_FACE('',(#1683),#10230,.F.);
#10735=ADVANCED_FACE('',(#1684),#10231,.F.);
#10736=ADVANCED_FACE('',(#1685,#854,#855,#856),#10232,.F.);
#10737=ADVANCED_FACE('',(#1686,#857),#1144,.F.);
#10738=ADVANCED_FACE('',(#1687,#858),#1145,.T.);
#10739=ADVANCED_FACE('',(#1688),#10233,.T.);
#10740=ADVANCED_FACE('',(#1689,#859),#1146,.F.);
#10741=ADVANCED_FACE('',(#1690,#860),#1147,.F.);
#10742=ADVANCED_FACE('',(#1691),#10234,.T.);
#10743=ADVANCED_FACE('',(#1692,#861),#1148,.T.);
#10744=ADVANCED_FACE('',(#1693),#10235,.F.);
#10745=ADVANCED_FACE('',(#1694),#10236,.T.);
#10746=ADVANCED_FACE('',(#1695),#10237,.F.);
#10747=ADVANCED_FACE('',(#1696),#10238,.T.);
#10748=ADVANCED_FACE('',(#1697),#10239,.F.);
#10749=ADVANCED_FACE('',(#1698),#10240,.T.);
#10750=ADVANCED_FACE('',(#1699),#10241,.F.);
#10751=ADVANCED_FACE('',(#1700),#10242,.T.);
#10752=ADVANCED_FACE('',(#1701),#10243,.F.);
#10753=ADVANCED_FACE('',(#1702),#10244,.T.);
#10754=ADVANCED_FACE('',(#1703),#10245,.F.);
#10755=ADVANCED_FACE('',(#1704),#10246,.T.);
#10756=ADVANCED_FACE('',(#1705),#10247,.F.);
#10757=ADVANCED_FACE('',(#1706),#10248,.T.);
#10758=ADVANCED_FACE('',(#1707),#10249,.F.);
#10759=ADVANCED_FACE('',(#1708),#10250,.T.);
#10760=ADVANCED_FACE('',(#1709),#10251,.F.);
#10761=ADVANCED_FACE('',(#1710),#10252,.T.);
#10762=ADVANCED_FACE('',(#1711),#10253,.F.);
#10763=ADVANCED_FACE('',(#1712),#10254,.T.);
#10764=ADVANCED_FACE('',(#1713),#10255,.F.);
#10765=ADVANCED_FACE('',(#1714),#10256,.T.);
#10766=ADVANCED_FACE('',(#1715),#10257,.F.);
#10767=ADVANCED_FACE('',(#1716),#10258,.T.);
#10768=ADVANCED_FACE('',(#1717),#10259,.F.);
#10769=ADVANCED_FACE('',(#1718),#10260,.T.);
#10770=ADVANCED_FACE('',(#1719),#10261,.F.);
#10771=ADVANCED_FACE('',(#1720),#10262,.T.);
#10772=ADVANCED_FACE('',(#1721),#10263,.F.);
#10773=ADVANCED_FACE('',(#1722),#10264,.T.);
#10774=ADVANCED_FACE('',(#1723),#10265,.F.);
#10775=ADVANCED_FACE('',(#1724),#10266,.T.);
#10776=ADVANCED_FACE('',(#1725),#10267,.F.);
#10777=ADVANCED_FACE('',(#1726),#10268,.T.);
#10778=ADVANCED_FACE('',(#1727),#10269,.F.);
#10779=ADVANCED_FACE('',(#1728),#10270,.T.);
#10780=ADVANCED_FACE('',(#1729),#10271,.F.);
#10781=ADVANCED_FACE('',(#1730),#10272,.T.);
#10782=ADVANCED_FACE('',(#1731),#10273,.F.);
#10783=ADVANCED_FACE('',(#1732),#10274,.T.);
#10784=ADVANCED_FACE('',(#1733),#10275,.F.);
#10785=ADVANCED_FACE('',(#1734,#862),#1149,.F.);
#10786=ADVANCED_FACE('',(#1735),#10276,.F.);
#10787=ADVANCED_FACE('',(#1736,#863),#1150,.F.);
#10788=ADVANCED_FACE('',(#1737),#10277,.F.);
#10789=ADVANCED_FACE('',(#1738),#10278,.F.);
#10790=ADVANCED_FACE('',(#1739),#10279,.F.);
#10791=ADVANCED_FACE('',(#1740),#10280,.F.);
#10792=ADVANCED_FACE('',(#1741),#10281,.F.);
#10793=ADVANCED_FACE('',(#1742),#10282,.F.);
#10794=ADVANCED_FACE('',(#1743),#1151,.T.);
#10795=ADVANCED_FACE('',(#1744),#1152,.T.);
#10796=ADVANCED_FACE('',(#1745),#1153,.T.);
#10797=ADVANCED_FACE('',(#1746),#1154,.T.);
#10798=ADVANCED_FACE('',(#1747,#864,#865,#866,#867,#868,#869),#1155,.T.);
#10799=ADVANCED_FACE('',(#1748,#870,#871,#872,#873,#874,#875),#1156,.F.);
#10800=ADVANCED_FACE('',(#1749),#10283,.F.);
#10801=ADVANCED_FACE('',(#1750),#1157,.F.);
#10802=ADVANCED_FACE('',(#1751),#10284,.F.);
#10803=ADVANCED_FACE('',(#1752),#1158,.F.);
#10804=ADVANCED_FACE('',(#1753),#1159,.F.);
#10805=ADVANCED_FACE('',(#1754),#10285,.F.);
#10806=ADVANCED_FACE('',(#1755),#10286,.F.);
#10807=ADVANCED_FACE('',(#1756),#1160,.F.);
#10808=ADVANCED_FACE('',(#1757),#1161,.T.);
#10809=ADVANCED_FACE('',(#1758),#1162,.T.);
#10810=ADVANCED_FACE('',(#1759),#10287,.F.);
#10811=ADVANCED_FACE('',(#1760),#1163,.T.);
#10812=ADVANCED_FACE('',(#1761),#10288,.F.);
#10813=ADVANCED_FACE('',(#1762),#1164,.T.);
#10814=ADVANCED_FACE('',(#1763,#876,#877),#1165,.T.);
#10815=ADVANCED_FACE('',(#1764),#1166,.T.);
#10816=ADVANCED_FACE('',(#1765),#1167,.F.);
#10817=ADVANCED_FACE('',(#1766),#1168,.T.);
#10818=ADVANCED_FACE('',(#1767),#1169,.T.);
#10819=ADVANCED_FACE('',(#1768,#878,#879),#1170,.F.);
#10820=ADVANCED_FACE('',(#1769),#1171,.T.);
#10821=ADVANCED_FACE('',(#1770),#1172,.T.);
#10822=ADVANCED_FACE('',(#1771),#1173,.T.);
#10823=ADVANCED_FACE('',(#1772),#1174,.T.);
#10824=ADVANCED_FACE('',(#1773),#1175,.T.);
#10825=ADVANCED_FACE('',(#1774),#1176,.F.);
#10826=ADVANCED_FACE('',(#1775),#1177,.T.);
#10827=ADVANCED_FACE('',(#1776),#10289,.F.);
#10828=ADVANCED_FACE('',(#1777),#1178,.T.);
#10829=ADVANCED_FACE('',(#1778),#10290,.F.);
#10830=ADVANCED_FACE('',(#1779),#1179,.T.);
#10831=ADVANCED_FACE('',(#1780),#10291,.F.);
#10832=ADVANCED_FACE('',(#1781),#1180,.T.);
#10833=ADVANCED_FACE('',(#1782),#10292,.F.);
#10834=ADVANCED_FACE('',(#1783),#1181,.T.);
#10835=ADVANCED_FACE('',(#1784),#1182,.T.);
#10836=ADVANCED_FACE('',(#1785),#1183,.T.);
#10837=ADVANCED_FACE('',(#1786),#1184,.T.);
#10838=ADVANCED_FACE('',(#1787),#1185,.T.);
#10839=ADVANCED_FACE('',(#1788,#880,#881,#882,#883),#1186,.T.);
#10840=ADVANCED_FACE('',(#1789),#1187,.T.);
#10841=ADVANCED_FACE('',(#1790),#1188,.T.);
#10842=ADVANCED_FACE('',(#1791),#1189,.T.);
#10843=ADVANCED_FACE('',(#1792),#1190,.T.);
#10844=ADVANCED_FACE('',(#1793),#1191,.T.);
#10845=ADVANCED_FACE('',(#1794),#1192,.T.);
#10846=ADVANCED_FACE('',(#1795),#1193,.T.);
#10847=ADVANCED_FACE('',(#1796),#1194,.T.);
#10848=ADVANCED_FACE('',(#1797),#1195,.T.);
#10849=ADVANCED_FACE('',(#1798),#1196,.T.);
#10850=ADVANCED_FACE('',(#1799),#1197,.T.);
#10851=ADVANCED_FACE('',(#1800),#1198,.T.);
#10852=ADVANCED_FACE('',(#1801),#1199,.T.);
#10853=ADVANCED_FACE('',(#1802),#1200,.T.);
#10854=ADVANCED_FACE('',(#1803),#1201,.T.);
#10855=ADVANCED_FACE('',(#1804),#1202,.T.);
#10856=ADVANCED_FACE('',(#1805),#1203,.T.);
#10857=ADVANCED_FACE('',(#1806),#1204,.F.);
#10858=ADVANCED_FACE('',(#1807),#1205,.T.);
#10859=ADVANCED_FACE('',(#1808),#1206,.T.);
#10860=ADVANCED_FACE('',(#1809),#1207,.T.);
#10861=ADVANCED_FACE('',(#1810),#1208,.T.);
#10862=ADVANCED_FACE('',(#1811),#1209,.T.);
#10863=ADVANCED_FACE('',(#1812),#1210,.T.);
#10864=ADVANCED_FACE('',(#1813),#1211,.T.);
#10865=ADVANCED_FACE('',(#1814),#1212,.T.);
#10866=ADVANCED_FACE('',(#1815),#1213,.T.);
#10867=ADVANCED_FACE('',(#1816),#1214,.T.);
#10868=ADVANCED_FACE('',(#1817),#504,.F.);
#10869=ADVANCED_FACE('',(#1818),#10293,.F.);
#10870=ADVANCED_FACE('',(#1819,#884),#1215,.T.);
#10871=ADVANCED_FACE('',(#1820),#10294,.T.);
#10872=ADVANCED_FACE('',(#1821,#885),#1216,.F.);
#10873=ADVANCED_FACE('',(#1822),#1217,.T.);
#10874=ADVANCED_FACE('',(#1823),#505,.T.);
#10875=ADVANCED_FACE('',(#1824),#10295,.T.);
#10876=ADVANCED_FACE('',(#1825),#506,.T.);
#10877=ADVANCED_FACE('',(#1826,#886),#1218,.T.);
#10878=ADVANCED_FACE('',(#1827),#507,.T.);
#10879=ADVANCED_FACE('',(#1828),#10296,.T.);
#10880=ADVANCED_FACE('',(#1829),#508,.T.);
#10881=ADVANCED_FACE('',(#1830),#1219,.T.);
#10882=ADVANCED_FACE('',(#1831),#1220,.F.);
#10883=ADVANCED_FACE('',(#1832),#1221,.F.);
#10884=ADVANCED_FACE('',(#1833),#1222,.F.);
#10885=ADVANCED_FACE('',(#1834),#1223,.F.);
#10886=ADVANCED_FACE('',(#1835),#1224,.F.);
#10887=ADVANCED_FACE('',(#1836),#1225,.F.);
#10888=ADVANCED_FACE('',(#1837),#1226,.F.);
#10889=ADVANCED_FACE('',(#1838),#1227,.F.);
#10890=ADVANCED_FACE('',(#1839),#1228,.F.);
#10891=ADVANCED_FACE('',(#1840),#1229,.F.);
#10892=ADVANCED_FACE('',(#1841),#1230,.F.);
#10893=ADVANCED_FACE('',(#1842),#1231,.F.);
#10894=ADVANCED_FACE('',(#1843),#1232,.F.);
#10895=ADVANCED_FACE('',(#1844),#1233,.F.);
#10896=ADVANCED_FACE('',(#1845),#1234,.F.);
#10897=ADVANCED_FACE('',(#1846),#1235,.F.);
#10898=ADVANCED_FACE('',(#1847),#1236,.F.);
#10899=ADVANCED_FACE('',(#1848),#1237,.T.);
#10900=ADVANCED_FACE('',(#1849),#509,.T.);
#10901=ADVANCED_FACE('',(#1850),#10297,.T.);
#10902=ADVANCED_FACE('',(#1851),#510,.T.);
#10903=ADVANCED_FACE('',(#1852,#887),#1238,.T.);
#10904=ADVANCED_FACE('',(#1853),#511,.T.);
#10905=ADVANCED_FACE('',(#1854),#10298,.T.);
#10906=ADVANCED_FACE('',(#1855),#1239,.T.);
#10907=ADVANCED_FACE('',(#1856),#512,.T.);
#10908=ADVANCED_FACE('',(#1857),#10299,.T.);
#10909=ADVANCED_FACE('',(#1858),#513,.T.);
#10910=ADVANCED_FACE('',(#1859,#888),#1240,.T.);
#10911=ADVANCED_FACE('',(#1860),#514,.T.);
#10912=ADVANCED_FACE('',(#1861),#10300,.T.);
#10913=ADVANCED_FACE('',(#1862),#515,.T.);
#10914=ADVANCED_FACE('',(#1863),#1241,.T.);
#10915=ADVANCED_FACE('',(#1864),#1242,.F.);
#10916=ADVANCED_FACE('',(#1865),#1243,.F.);
#10917=ADVANCED_FACE('',(#1866),#1244,.F.);
#10918=ADVANCED_FACE('',(#1867),#1245,.F.);
#10919=ADVANCED_FACE('',(#1868),#1246,.F.);
#10920=ADVANCED_FACE('',(#1869),#1247,.F.);
#10921=ADVANCED_FACE('',(#1870),#1248,.F.);
#10922=ADVANCED_FACE('',(#1871),#1249,.F.);
#10923=CLOSED_SHELL('',(#10301,#10302,#10303,#10304,#10305,#10306,#10307,
#10308,#10309,#10310,#10311,#10312,#10313,#10314,#10315,#10316,#10317,#10318,
#10319,#10320,#10321,#10322,#10323,#10324,#10325,#10326,#10327,#10328,#10329,
#10330,#10331,#10332,#10333,#10334,#10335,#10336,#10337,#10338,#10339,#10340,
#10341,#10342));
#10924=CLOSED_SHELL('',(#10343,#10344,#10345,#10346,#10347,#10348));
#10925=CLOSED_SHELL('',(#10349,#10350,#10351,#10352,#10353,#10354));
#10926=CLOSED_SHELL('',(#10355,#10356,#10357,#10358,#10359,#10360));
#10927=CLOSED_SHELL('',(#10361,#10362,#10363,#10364,#10365,#10366));
#10928=CLOSED_SHELL('',(#10367,#10368,#10369,#10370,#10371,#10372,#10373,
#10374,#10375,#10376,#10377,#10378,#10379,#10380,#10381,#10382,#10383,#10384,
#10385));
#10929=CLOSED_SHELL('',(#10386,#10387,#10388,#10389));
#10930=CLOSED_SHELL('',(#10390,#10391,#10392,#10393,#10394,#10395,#10396,
#10397,#10398,#10399,#10400,#10401,#10402));
#10931=CLOSED_SHELL('',(#10403,#10404,#10405,#10406,#10407,#10408,#10409,
#10410,#10411,#10412,#10413,#10414,#10415));
#10932=CLOSED_SHELL('',(#10416,#10417,#10418,#10419,#10420,#10421,#10422,
#10423,#10424,#10425,#10426,#10427,#10428,#10429,#10430,#10431,#10432,#10433,
#10434));
#10933=CLOSED_SHELL('',(#10435,#10436,#10437,#10438));
#10934=CLOSED_SHELL('',(#10439,#10440,#10441,#10442,#10443,#10444,#10445,
#10446,#10447,#10448,#10449,#10450,#10451));
#10935=CLOSED_SHELL('',(#10452,#10453,#10454,#10455,#10456,#10457,#10458,
#10459,#10460,#10461,#10462,#10463,#10464));
#10936=CLOSED_SHELL('',(#10465,#10466,#10467,#10468,#10469,#10470,#10471,
#10472,#10473,#10474));
#10937=CLOSED_SHELL('',(#10475,#10476,#10477,#10478,#10479,#10480,#10481,
#10482,#10483,#10484,#10485,#10486,#10487,#10488,#10489,#10490,#10491,#10492,
#10493,#10494));
#10938=CLOSED_SHELL('',(#10495,#10496,#10497,#10498,#10499,#10500,#10501,
#10502,#10503,#10504,#10505,#10506,#10507,#10508,#10509,#10510,#10511,#10512,
#10513,#10514));
#10939=CLOSED_SHELL('',(#10515,#10516,#10517,#10518,#10519,#10520,#10521,
#10522));
#10940=CLOSED_SHELL('',(#10523,#10524,#10525,#10526,#10527,#10528,#10529,
#10530));
#10941=CLOSED_SHELL('',(#10531));
#10942=CLOSED_SHELL('',(#10532));
#10943=CLOSED_SHELL('',(#10533));
#10944=CLOSED_SHELL('',(#10534));
#10945=CLOSED_SHELL('',(#10535));
#10946=CLOSED_SHELL('',(#10536));
#10947=CLOSED_SHELL('',(#10537));
#10948=CLOSED_SHELL('',(#10538));
#10949=CLOSED_SHELL('',(#10539,#10540,#10541,#10542,#10543,#10544,#10545,
#10546,#10547,#10548,#10549,#10550,#10551,#10552,#10553,#10554,#10555,#10556,
#10557));
#10950=CLOSED_SHELL('',(#10558,#10559,#10560,#10561));
#10951=CLOSED_SHELL('',(#10562,#10563,#10564,#10565));
#10952=CLOSED_SHELL('',(#10566,#10567,#10568,#10569,#10570,#10571,#10572,
#10573,#10574,#10575,#10576,#10577,#10578,#10579,#10580,#10581,#10582,#10583,
#10584,#10585,#10586,#10587,#10588,#10589,#10590,#10591,#10592,#10593,#10594,
#10595,#10596,#10597,#10598,#10599,#10600,#10601,#10602,#10603,#10604,#10605,
#10606,#10607,#10608,#10609,#10610,#10611,#10612));
#10953=CLOSED_SHELL('',(#10613,#10614,#10615,#10616,#10617,#10618,#10619,
#10620,#10621,#10622,#10623,#10624,#10625,#10626));
#10954=CLOSED_SHELL('',(#10627,#10628,#10629,#10630,#10631,#10632,#10633,
#10634));
#10955=CLOSED_SHELL('',(#10635,#10636,#10637,#10638,#10639,#10640,#10641,
#10642));
#10956=CLOSED_SHELL('',(#10643,#10644,#10645,#10646,#10647,#10648,#10649,
#10650,#10651,#10652,#10653,#10654,#10655,#10656,#10657,#10658,#10659,#10660,
#10661,#10662,#10663,#10664,#10665,#10666,#10667,#10668));
#10957=CLOSED_SHELL('',(#10669,#10670,#10671,#10672,#10673,#10674,#10675,
#10676,#10677,#10678,#10679));
#10958=CLOSED_SHELL('',(#10680,#10681,#10682,#10683,#10684,#10685));
#10959=CLOSED_SHELL('',(#10686,#10687,#10688,#10689));
#10960=CLOSED_SHELL('',(#10690,#10691,#10692));
#10961=CLOSED_SHELL('',(#10693,#10694,#10695));
#10962=CLOSED_SHELL('',(#10696,#10697,#10698,#10699));
#10963=CLOSED_SHELL('',(#10700,#10701,#10702,#10703,#10704,#10705,#10706,
#10707,#10708,#10709,#10710));
#10964=CLOSED_SHELL('',(#10711,#10712,#10713,#10714,#10715,#10716));
#10965=CLOSED_SHELL('',(#10717,#10718,#10719,#10720));
#10966=CLOSED_SHELL('',(#10721,#10722,#10723));
#10967=CLOSED_SHELL('',(#10724,#10725,#10726));
#10968=CLOSED_SHELL('',(#10727,#10728,#10729,#10730));
#10969=CLOSED_SHELL('',(#10731,#10732,#10733,#10734,#10735,#10736,#10737,
#10738,#10739,#10740,#10741,#10742,#10743,#10744,#10745,#10746,#10747,#10748,
#10749,#10750,#10751,#10752,#10753,#10754,#10755,#10756,#10757,#10758,#10759,
#10760,#10761,#10762,#10763,#10764,#10765,#10766,#10767,#10768,#10769,#10770,
#10771,#10772,#10773,#10774,#10775,#10776,#10777,#10778,#10779,#10780,#10781,
#10782,#10783));
#10970=CLOSED_SHELL('',(#10784,#10785,#10786,#10787,#10788,#10789,#10790,
#10791,#10792,#10793,#10794,#10795,#10796,#10797,#10798,#10799));
#10971=CLOSED_SHELL('',(#10800,#10801,#10802,#10803,#10804,#10805,#10806,
#10807,#10808,#10809,#10810,#10811,#10812,#10813,#10814,#10815,#10816,#10817,
#10818,#10819));
#10972=CLOSED_SHELL('',(#10820,#10821,#10822,#10823,#10824,#10825));
#10973=CLOSED_SHELL('',(#10826,#10827,#10828,#10829,#10830,#10831,#10832,
#10833,#10834,#10835,#10836,#10837,#10838,#10839,#10840,#10841,#10842,#10843,
#10844,#10845,#10846,#10847));
#10974=CLOSED_SHELL('',(#10848,#10849,#10850,#10851,#10852,#10853,#10854,
#10855,#10856,#10857));
#10975=CLOSED_SHELL('',(#10858,#10859,#10860,#10861,#10862,#10863,#10864,
#10865,#10866,#10867));
#10976=CLOSED_SHELL('',(#10868,#10869,#10870,#10871,#10872));
#10977=CLOSED_SHELL('',(#10873,#10874,#10875,#10876,#10877,#10878,#10879,
#10880,#10881));
#10978=CLOSED_SHELL('',(#10882,#10883,#10884,#10885,#10886,#10887,#10888,
#10889));
#10979=CLOSED_SHELL('',(#10890,#10891,#10892,#10893,#10894,#10895,#10896,
#10897));
#10980=CLOSED_SHELL('',(#10898,#10899,#10900,#10901,#10902,#10903,#10904,
#10905));
#10981=CLOSED_SHELL('',(#10906,#10907,#10908,#10909,#10910,#10911,#10912,
#10913,#10914));
#10982=CLOSED_SHELL('',(#10915,#10916,#10917,#10918,#10919,#10920,#10921,
#10922));
#10983=DERIVED_UNIT_ELEMENT(#11075,1.);
#10984=DERIVED_UNIT_ELEMENT(#20098,-3.);
#10985=DERIVED_UNIT_ELEMENT(#11075,1.);
#10986=DERIVED_UNIT_ELEMENT(#20098,-3.);
#10987=DERIVED_UNIT_ELEMENT(#11075,1.);
#10988=DERIVED_UNIT_ELEMENT(#20098,-3.);
#10989=DERIVED_UNIT_ELEMENT(#11075,1.);
#10990=DERIVED_UNIT_ELEMENT(#20098,-3.);
#10991=DERIVED_UNIT_ELEMENT(#11075,1.);
#10992=DERIVED_UNIT_ELEMENT(#20098,-3.);
#10993=DERIVED_UNIT_ELEMENT(#11075,1.);
#10994=DERIVED_UNIT_ELEMENT(#20098,-3.);
#10995=DERIVED_UNIT_ELEMENT(#11075,1.);
#10996=DERIVED_UNIT_ELEMENT(#20098,-3.);
#10997=DERIVED_UNIT_ELEMENT(#11075,1.);
#10998=DERIVED_UNIT_ELEMENT(#20098,-3.);
#10999=DERIVED_UNIT_ELEMENT(#11075,1.);
#11000=DERIVED_UNIT_ELEMENT(#20098,-3.);
#11001=DERIVED_UNIT_ELEMENT(#11075,1.);
#11002=DERIVED_UNIT_ELEMENT(#20098,-3.);
#11003=DERIVED_UNIT_ELEMENT(#11075,1.);
#11004=DERIVED_UNIT_ELEMENT(#20098,-3.);
#11005=DERIVED_UNIT_ELEMENT(#11075,1.);
#11006=DERIVED_UNIT_ELEMENT(#20098,-3.);
#11007=DERIVED_UNIT_ELEMENT(#11075,1.);
#11008=DERIVED_UNIT_ELEMENT(#20098,-3.);
#11009=DERIVED_UNIT_ELEMENT(#11075,1.);
#11010=DERIVED_UNIT_ELEMENT(#20098,-3.);
#11011=DERIVED_UNIT_ELEMENT(#11075,1.);
#11012=DERIVED_UNIT_ELEMENT(#20098,-3.);
#11013=DERIVED_UNIT_ELEMENT(#11075,1.);
#11014=DERIVED_UNIT_ELEMENT(#20098,-3.);
#11015=DERIVED_UNIT_ELEMENT(#11075,1.);
#11016=DERIVED_UNIT_ELEMENT(#20098,-3.);
#11017=DERIVED_UNIT_ELEMENT(#11075,1.);
#11018=DERIVED_UNIT_ELEMENT(#20098,-3.);
#11019=DERIVED_UNIT_ELEMENT(#11075,1.);
#11020=DERIVED_UNIT_ELEMENT(#20098,-3.);
#11021=DERIVED_UNIT_ELEMENT(#11075,1.);
#11022=DERIVED_UNIT_ELEMENT(#20098,-3.);
#11023=DERIVED_UNIT_ELEMENT(#11075,1.);
#11024=DERIVED_UNIT_ELEMENT(#20098,-3.);
#11025=DERIVED_UNIT_ELEMENT(#11075,1.);
#11026=DERIVED_UNIT_ELEMENT(#20098,-3.);
#11027=DERIVED_UNIT_ELEMENT(#11075,1.);
#11028=DERIVED_UNIT_ELEMENT(#20098,-3.);
#11029=DERIVED_UNIT_ELEMENT(#11075,1.);
#11030=DERIVED_UNIT_ELEMENT(#20098,-3.);
#11031=DERIVED_UNIT_ELEMENT(#11075,1.);
#11032=DERIVED_UNIT_ELEMENT(#20098,-3.);
#11033=DERIVED_UNIT_ELEMENT(#11075,1.);
#11034=DERIVED_UNIT_ELEMENT(#20098,-3.);
#11035=DERIVED_UNIT_ELEMENT(#11075,1.);
#11036=DERIVED_UNIT_ELEMENT(#20098,-3.);
#11037=DERIVED_UNIT_ELEMENT(#11075,1.);
#11038=DERIVED_UNIT_ELEMENT(#20098,-3.);
#11039=DERIVED_UNIT_ELEMENT(#11075,1.);
#11040=DERIVED_UNIT_ELEMENT(#20098,-3.);
#11041=DERIVED_UNIT_ELEMENT(#11075,1.);
#11042=DERIVED_UNIT_ELEMENT(#20098,-3.);
#11043=DERIVED_UNIT_ELEMENT(#11075,1.);
#11044=DERIVED_UNIT_ELEMENT(#20098,-3.);
#11045=DERIVED_UNIT_ELEMENT(#11075,1.);
#11046=DERIVED_UNIT_ELEMENT(#20098,-3.);
#11047=DERIVED_UNIT_ELEMENT(#11075,1.);
#11048=DERIVED_UNIT_ELEMENT(#20098,-3.);
#11049=DERIVED_UNIT_ELEMENT(#11075,1.);
#11050=DERIVED_UNIT_ELEMENT(#20098,-3.);
#11051=DERIVED_UNIT_ELEMENT(#11075,1.);
#11052=DERIVED_UNIT_ELEMENT(#20098,-3.);
#11053=DERIVED_UNIT_ELEMENT(#11075,1.);
#11054=DERIVED_UNIT_ELEMENT(#20098,-3.);
#11055=DERIVED_UNIT_ELEMENT(#11075,1.);
#11056=DERIVED_UNIT_ELEMENT(#20098,-3.);
#11057=DERIVED_UNIT_ELEMENT(#11075,1.);
#11058=DERIVED_UNIT_ELEMENT(#20098,-3.);
#11059=DERIVED_UNIT_ELEMENT(#11075,1.);
#11060=DERIVED_UNIT_ELEMENT(#20098,-3.);
#11061=DERIVED_UNIT_ELEMENT(#11075,1.);
#11062=DERIVED_UNIT_ELEMENT(#20098,-3.);
#11063=DERIVED_UNIT_ELEMENT(#11075,1.);
#11064=DERIVED_UNIT_ELEMENT(#20098,-3.);
#11065=DERIVED_UNIT_ELEMENT(#11075,1.);
#11066=DERIVED_UNIT_ELEMENT(#20098,-3.);
#11067=DERIVED_UNIT_ELEMENT(#11075,1.);
#11068=DERIVED_UNIT_ELEMENT(#20098,-3.);
#11069=DERIVED_UNIT_ELEMENT(#11075,1.);
#11070=DERIVED_UNIT_ELEMENT(#20098,-3.);
#11071=DERIVED_UNIT_ELEMENT(#11075,1.);
#11072=DERIVED_UNIT_ELEMENT(#20098,-3.);
#11073=DERIVED_UNIT_ELEMENT(#11075,1.);
#11074=DERIVED_UNIT_ELEMENT(#20098,-3.);
#11075=(
MASS_UNIT()
NAMED_UNIT(*)
SI_UNIT(.KILO.,.GRAM.)
);
#11076=DERIVED_UNIT((#10983,#10984));
#11077=DERIVED_UNIT((#10985,#10986));
#11078=DERIVED_UNIT((#10987,#10988));
#11079=DERIVED_UNIT((#10989,#10990));
#11080=DERIVED_UNIT((#10991,#10992));
#11081=DERIVED_UNIT((#10993,#10994));
#11082=DERIVED_UNIT((#10995,#10996));
#11083=DERIVED_UNIT((#10997,#10998));
#11084=DERIVED_UNIT((#10999,#11000));
#11085=DERIVED_UNIT((#11001,#11002));
#11086=DERIVED_UNIT((#11003,#11004));
#11087=DERIVED_UNIT((#11005,#11006));
#11088=DERIVED_UNIT((#11007,#11008));
#11089=DERIVED_UNIT((#11009,#11010));
#11090=DERIVED_UNIT((#11011,#11012));
#11091=DERIVED_UNIT((#11013,#11014));
#11092=DERIVED_UNIT((#11015,#11016));
#11093=DERIVED_UNIT((#11017,#11018));
#11094=DERIVED_UNIT((#11019,#11020));
#11095=DERIVED_UNIT((#11021,#11022));
#11096=DERIVED_UNIT((#11023,#11024));
#11097=DERIVED_UNIT((#11025,#11026));
#11098=DERIVED_UNIT((#11027,#11028));
#11099=DERIVED_UNIT((#11029,#11030));
#11100=DERIVED_UNIT((#11031,#11032));
#11101=DERIVED_UNIT((#11033,#11034));
#11102=DERIVED_UNIT((#11035,#11036));
#11103=DERIVED_UNIT((#11037,#11038));
#11104=DERIVED_UNIT((#11039,#11040));
#11105=DERIVED_UNIT((#11041,#11042));
#11106=DERIVED_UNIT((#11043,#11044));
#11107=DERIVED_UNIT((#11045,#11046));
#11108=DERIVED_UNIT((#11047,#11048));
#11109=DERIVED_UNIT((#11049,#11050));
#11110=DERIVED_UNIT((#11051,#11052));
#11111=DERIVED_UNIT((#11053,#11054));
#11112=DERIVED_UNIT((#11055,#11056));
#11113=DERIVED_UNIT((#11057,#11058));
#11114=DERIVED_UNIT((#11059,#11060));
#11115=DERIVED_UNIT((#11061,#11062));
#11116=DERIVED_UNIT((#11063,#11064));
#11117=DERIVED_UNIT((#11065,#11066));
#11118=DERIVED_UNIT((#11067,#11068));
#11119=DERIVED_UNIT((#11069,#11070));
#11120=DERIVED_UNIT((#11071,#11072));
#11121=DERIVED_UNIT((#11073,#11074));
#11122=MEASURE_REPRESENTATION_ITEM('density measure',
POSITIVE_RATIO_MEASURE(7850.),#11076);
#11123=MEASURE_REPRESENTATION_ITEM('density measure',
POSITIVE_RATIO_MEASURE(7850.),#11077);
#11124=MEASURE_REPRESENTATION_ITEM('density measure',
POSITIVE_RATIO_MEASURE(7850.),#11078);
#11125=MEASURE_REPRESENTATION_ITEM('density measure',
POSITIVE_RATIO_MEASURE(7850.),#11079);
#11126=MEASURE_REPRESENTATION_ITEM('density measure',
POSITIVE_RATIO_MEASURE(7850.),#11080);
#11127=MEASURE_REPRESENTATION_ITEM('density measure',
POSITIVE_RATIO_MEASURE(7850.),#11081);
#11128=MEASURE_REPRESENTATION_ITEM('density measure',
POSITIVE_RATIO_MEASURE(7850.),#11082);
#11129=MEASURE_REPRESENTATION_ITEM('density measure',
POSITIVE_RATIO_MEASURE(7850.),#11083);
#11130=MEASURE_REPRESENTATION_ITEM('density measure',
POSITIVE_RATIO_MEASURE(7850.),#11084);
#11131=MEASURE_REPRESENTATION_ITEM('density measure',
POSITIVE_RATIO_MEASURE(7850.),#11085);
#11132=MEASURE_REPRESENTATION_ITEM('density measure',
POSITIVE_RATIO_MEASURE(7850.),#11086);
#11133=MEASURE_REPRESENTATION_ITEM('density measure',
POSITIVE_RATIO_MEASURE(7850.),#11087);
#11134=MEASURE_REPRESENTATION_ITEM('density measure',
POSITIVE_RATIO_MEASURE(7850.),#11088);
#11135=MEASURE_REPRESENTATION_ITEM('density measure',
POSITIVE_RATIO_MEASURE(7850.),#11089);
#11136=MEASURE_REPRESENTATION_ITEM('density measure',
POSITIVE_RATIO_MEASURE(7850.),#11090);
#11137=MEASURE_REPRESENTATION_ITEM('density measure',
POSITIVE_RATIO_MEASURE(7850.),#11091);
#11138=MEASURE_REPRESENTATION_ITEM('density measure',
POSITIVE_RATIO_MEASURE(7850.),#11092);
#11139=MEASURE_REPRESENTATION_ITEM('density measure',
POSITIVE_RATIO_MEASURE(7850.),#11093);
#11140=MEASURE_REPRESENTATION_ITEM('density measure',
POSITIVE_RATIO_MEASURE(7850.),#11094);
#11141=MEASURE_REPRESENTATION_ITEM('density measure',
POSITIVE_RATIO_MEASURE(7850.),#11095);
#11142=MEASURE_REPRESENTATION_ITEM('density measure',
POSITIVE_RATIO_MEASURE(7850.),#11096);
#11143=MEASURE_REPRESENTATION_ITEM('density measure',
POSITIVE_RATIO_MEASURE(7850.),#11097);
#11144=MEASURE_REPRESENTATION_ITEM('density measure',
POSITIVE_RATIO_MEASURE(7850.),#11098);
#11145=MEASURE_REPRESENTATION_ITEM('density measure',
POSITIVE_RATIO_MEASURE(7850.),#11099);
#11146=MEASURE_REPRESENTATION_ITEM('density measure',
POSITIVE_RATIO_MEASURE(7850.),#11100);
#11147=MEASURE_REPRESENTATION_ITEM('density measure',
POSITIVE_RATIO_MEASURE(7850.),#11101);
#11148=MEASURE_REPRESENTATION_ITEM('density measure',
POSITIVE_RATIO_MEASURE(7850.),#11102);
#11149=MEASURE_REPRESENTATION_ITEM('density measure',
POSITIVE_RATIO_MEASURE(7850.),#11103);
#11150=MEASURE_REPRESENTATION_ITEM('density measure',
POSITIVE_RATIO_MEASURE(7850.),#11104);
#11151=MEASURE_REPRESENTATION_ITEM('density measure',
POSITIVE_RATIO_MEASURE(7850.),#11105);
#11152=MEASURE_REPRESENTATION_ITEM('density measure',
POSITIVE_RATIO_MEASURE(7850.),#11106);
#11153=MEASURE_REPRESENTATION_ITEM('density measure',
POSITIVE_RATIO_MEASURE(7850.),#11107);
#11154=MEASURE_REPRESENTATION_ITEM('density measure',
POSITIVE_RATIO_MEASURE(7850.),#11108);
#11155=MEASURE_REPRESENTATION_ITEM('density measure',
POSITIVE_RATIO_MEASURE(7850.),#11109);
#11156=MEASURE_REPRESENTATION_ITEM('density measure',
POSITIVE_RATIO_MEASURE(7850.),#11110);
#11157=MEASURE_REPRESENTATION_ITEM('density measure',
POSITIVE_RATIO_MEASURE(7850.),#11111);
#11158=MEASURE_REPRESENTATION_ITEM('density measure',
POSITIVE_RATIO_MEASURE(7850.),#11112);
#11159=MEASURE_REPRESENTATION_ITEM('density measure',
POSITIVE_RATIO_MEASURE(7850.),#11113);
#11160=MEASURE_REPRESENTATION_ITEM('density measure',
POSITIVE_RATIO_MEASURE(7850.),#11114);
#11161=MEASURE_REPRESENTATION_ITEM('density measure',
POSITIVE_RATIO_MEASURE(7850.),#11115);
#11162=MEASURE_REPRESENTATION_ITEM('density measure',
POSITIVE_RATIO_MEASURE(7850.),#11116);
#11163=MEASURE_REPRESENTATION_ITEM('density measure',
POSITIVE_RATIO_MEASURE(7850.),#11117);
#11164=MEASURE_REPRESENTATION_ITEM('density measure',
POSITIVE_RATIO_MEASURE(7850.),#11118);
#11165=MEASURE_REPRESENTATION_ITEM('density measure',
POSITIVE_RATIO_MEASURE(7850.),#11119);
#11166=MEASURE_REPRESENTATION_ITEM('density measure',
POSITIVE_RATIO_MEASURE(7850.),#11120);
#11167=MEASURE_REPRESENTATION_ITEM('density measure',
POSITIVE_RATIO_MEASURE(7850.),#11121);
#11168=PROPERTY_DEFINITION_REPRESENTATION(#11398,#11260);
#11169=PROPERTY_DEFINITION_REPRESENTATION(#11399,#11261);
#11170=PROPERTY_DEFINITION_REPRESENTATION(#11400,#11262);
#11171=PROPERTY_DEFINITION_REPRESENTATION(#11401,#11263);
#11172=PROPERTY_DEFINITION_REPRESENTATION(#11402,#11264);
#11173=PROPERTY_DEFINITION_REPRESENTATION(#11403,#11265);
#11174=PROPERTY_DEFINITION_REPRESENTATION(#11404,#11266);
#11175=PROPERTY_DEFINITION_REPRESENTATION(#11405,#11267);
#11176=PROPERTY_DEFINITION_REPRESENTATION(#11406,#11268);
#11177=PROPERTY_DEFINITION_REPRESENTATION(#11407,#11269);
#11178=PROPERTY_DEFINITION_REPRESENTATION(#11408,#11270);
#11179=PROPERTY_DEFINITION_REPRESENTATION(#11409,#11271);
#11180=PROPERTY_DEFINITION_REPRESENTATION(#11410,#11272);
#11181=PROPERTY_DEFINITION_REPRESENTATION(#11411,#11273);
#11182=PROPERTY_DEFINITION_REPRESENTATION(#11412,#11274);
#11183=PROPERTY_DEFINITION_REPRESENTATION(#11413,#11275);
#11184=PROPERTY_DEFINITION_REPRESENTATION(#11414,#11276);
#11185=PROPERTY_DEFINITION_REPRESENTATION(#11415,#11277);
#11186=PROPERTY_DEFINITION_REPRESENTATION(#11416,#11278);
#11187=PROPERTY_DEFINITION_REPRESENTATION(#11417,#11279);
#11188=PROPERTY_DEFINITION_REPRESENTATION(#11418,#11280);
#11189=PROPERTY_DEFINITION_REPRESENTATION(#11419,#11281);
#11190=PROPERTY_DEFINITION_REPRESENTATION(#11420,#11282);
#11191=PROPERTY_DEFINITION_REPRESENTATION(#11421,#11283);
#11192=PROPERTY_DEFINITION_REPRESENTATION(#11422,#11284);
#11193=PROPERTY_DEFINITION_REPRESENTATION(#11423,#11285);
#11194=PROPERTY_DEFINITION_REPRESENTATION(#11424,#11286);
#11195=PROPERTY_DEFINITION_REPRESENTATION(#11425,#11287);
#11196=PROPERTY_DEFINITION_REPRESENTATION(#11426,#11288);
#11197=PROPERTY_DEFINITION_REPRESENTATION(#11427,#11289);
#11198=PROPERTY_DEFINITION_REPRESENTATION(#11428,#11290);
#11199=PROPERTY_DEFINITION_REPRESENTATION(#11429,#11291);
#11200=PROPERTY_DEFINITION_REPRESENTATION(#11430,#11292);
#11201=PROPERTY_DEFINITION_REPRESENTATION(#11431,#11293);
#11202=PROPERTY_DEFINITION_REPRESENTATION(#11432,#11294);
#11203=PROPERTY_DEFINITION_REPRESENTATION(#11433,#11295);
#11204=PROPERTY_DEFINITION_REPRESENTATION(#11434,#11296);
#11205=PROPERTY_DEFINITION_REPRESENTATION(#11435,#11297);
#11206=PROPERTY_DEFINITION_REPRESENTATION(#11436,#11298);
#11207=PROPERTY_DEFINITION_REPRESENTATION(#11437,#11299);
#11208=PROPERTY_DEFINITION_REPRESENTATION(#11438,#11300);
#11209=PROPERTY_DEFINITION_REPRESENTATION(#11439,#11301);
#11210=PROPERTY_DEFINITION_REPRESENTATION(#11440,#11302);
#11211=PROPERTY_DEFINITION_REPRESENTATION(#11441,#11303);
#11212=PROPERTY_DEFINITION_REPRESENTATION(#11442,#11304);
#11213=PROPERTY_DEFINITION_REPRESENTATION(#11443,#11305);
#11214=PROPERTY_DEFINITION_REPRESENTATION(#11444,#11306);
#11215=PROPERTY_DEFINITION_REPRESENTATION(#11445,#11307);
#11216=PROPERTY_DEFINITION_REPRESENTATION(#11446,#11308);
#11217=PROPERTY_DEFINITION_REPRESENTATION(#11447,#11309);
#11218=PROPERTY_DEFINITION_REPRESENTATION(#11448,#11310);
#11219=PROPERTY_DEFINITION_REPRESENTATION(#11449,#11311);
#11220=PROPERTY_DEFINITION_REPRESENTATION(#11450,#11312);
#11221=PROPERTY_DEFINITION_REPRESENTATION(#11451,#11313);
#11222=PROPERTY_DEFINITION_REPRESENTATION(#11452,#11314);
#11223=PROPERTY_DEFINITION_REPRESENTATION(#11453,#11315);
#11224=PROPERTY_DEFINITION_REPRESENTATION(#11454,#11316);
#11225=PROPERTY_DEFINITION_REPRESENTATION(#11455,#11317);
#11226=PROPERTY_DEFINITION_REPRESENTATION(#11456,#11318);
#11227=PROPERTY_DEFINITION_REPRESENTATION(#11457,#11319);
#11228=PROPERTY_DEFINITION_REPRESENTATION(#11458,#11320);
#11229=PROPERTY_DEFINITION_REPRESENTATION(#11459,#11321);
#11230=PROPERTY_DEFINITION_REPRESENTATION(#11460,#11322);
#11231=PROPERTY_DEFINITION_REPRESENTATION(#11461,#11323);
#11232=PROPERTY_DEFINITION_REPRESENTATION(#11462,#11324);
#11233=PROPERTY_DEFINITION_REPRESENTATION(#11463,#11325);
#11234=PROPERTY_DEFINITION_REPRESENTATION(#11464,#11326);
#11235=PROPERTY_DEFINITION_REPRESENTATION(#11465,#11327);
#11236=PROPERTY_DEFINITION_REPRESENTATION(#11466,#11328);
#11237=PROPERTY_DEFINITION_REPRESENTATION(#11467,#11329);
#11238=PROPERTY_DEFINITION_REPRESENTATION(#11468,#11330);
#11239=PROPERTY_DEFINITION_REPRESENTATION(#11469,#11331);
#11240=PROPERTY_DEFINITION_REPRESENTATION(#11470,#11332);
#11241=PROPERTY_DEFINITION_REPRESENTATION(#11471,#11333);
#11242=PROPERTY_DEFINITION_REPRESENTATION(#11472,#11334);
#11243=PROPERTY_DEFINITION_REPRESENTATION(#11473,#11335);
#11244=PROPERTY_DEFINITION_REPRESENTATION(#11474,#11336);
#11245=PROPERTY_DEFINITION_REPRESENTATION(#11475,#11337);
#11246=PROPERTY_DEFINITION_REPRESENTATION(#11476,#11338);
#11247=PROPERTY_DEFINITION_REPRESENTATION(#11477,#11339);
#11248=PROPERTY_DEFINITION_REPRESENTATION(#11478,#11340);
#11249=PROPERTY_DEFINITION_REPRESENTATION(#11479,#11341);
#11250=PROPERTY_DEFINITION_REPRESENTATION(#11480,#11342);
#11251=PROPERTY_DEFINITION_REPRESENTATION(#11481,#11343);
#11252=PROPERTY_DEFINITION_REPRESENTATION(#11482,#11344);
#11253=PROPERTY_DEFINITION_REPRESENTATION(#11483,#11345);
#11254=PROPERTY_DEFINITION_REPRESENTATION(#11484,#11346);
#11255=PROPERTY_DEFINITION_REPRESENTATION(#11485,#11347);
#11256=PROPERTY_DEFINITION_REPRESENTATION(#11486,#11348);
#11257=PROPERTY_DEFINITION_REPRESENTATION(#11487,#11349);
#11258=PROPERTY_DEFINITION_REPRESENTATION(#11488,#11350);
#11259=PROPERTY_DEFINITION_REPRESENTATION(#11489,#11351);
#11260=REPRESENTATION('material name',(#11352),#20045);
#11261=REPRESENTATION('density',(#11122),#20045);
#11262=REPRESENTATION('material name',(#11353),#20046);
#11263=REPRESENTATION('density',(#11123),#20046);
#11264=REPRESENTATION('material name',(#11354),#20047);
#11265=REPRESENTATION('density',(#11124),#20047);
#11266=REPRESENTATION('material name',(#11355),#20048);
#11267=REPRESENTATION('density',(#11125),#20048);
#11268=REPRESENTATION('material name',(#11356),#20049);
#11269=REPRESENTATION('density',(#11126),#20049);
#11270=REPRESENTATION('material name',(#11357),#20050);
#11271=REPRESENTATION('density',(#11127),#20050);
#11272=REPRESENTATION('material name',(#11358),#20051);
#11273=REPRESENTATION('density',(#11128),#20051);
#11274=REPRESENTATION('material name',(#11359),#20052);
#11275=REPRESENTATION('density',(#11129),#20052);
#11276=REPRESENTATION('material name',(#11360),#20053);
#11277=REPRESENTATION('density',(#11130),#20053);
#11278=REPRESENTATION('material name',(#11361),#20054);
#11279=REPRESENTATION('density',(#11131),#20054);
#11280=REPRESENTATION('material name',(#11362),#20055);
#11281=REPRESENTATION('density',(#11132),#20055);
#11282=REPRESENTATION('material name',(#11363),#20056);
#11283=REPRESENTATION('density',(#11133),#20056);
#11284=REPRESENTATION('material name',(#11364),#20057);
#11285=REPRESENTATION('density',(#11134),#20057);
#11286=REPRESENTATION('material name',(#11365),#20058);
#11287=REPRESENTATION('density',(#11135),#20058);
#11288=REPRESENTATION('material name',(#11366),#20060);
#11289=REPRESENTATION('density',(#11136),#20060);
#11290=REPRESENTATION('material name',(#11367),#20061);
#11291=REPRESENTATION('density',(#11137),#20061);
#11292=REPRESENTATION('material name',(#11368),#20062);
#11293=REPRESENTATION('density',(#11138),#20062);
#11294=REPRESENTATION('material name',(#11369),#20063);
#11295=REPRESENTATION('density',(#11139),#20063);
#11296=REPRESENTATION('material name',(#11370),#20064);
#11297=REPRESENTATION('density',(#11140),#20064);
#11298=REPRESENTATION('material name',(#11371),#20065);
#11299=REPRESENTATION('density',(#11141),#20065);
#11300=REPRESENTATION('material name',(#11372),#20066);
#11301=REPRESENTATION('density',(#11142),#20066);
#11302=REPRESENTATION('material name',(#11373),#20067);
#11303=REPRESENTATION('density',(#11143),#20067);
#11304=REPRESENTATION('material name',(#11374),#20068);
#11305=REPRESENTATION('density',(#11144),#20068);
#11306=REPRESENTATION('material name',(#11375),#20070);
#11307=REPRESENTATION('density',(#11145),#20070);
#11308=REPRESENTATION('material name',(#11376),#20071);
#11309=REPRESENTATION('density',(#11146),#20071);
#11310=REPRESENTATION('material name',(#11377),#20072);
#11311=REPRESENTATION('density',(#11147),#20072);
#11312=REPRESENTATION('material name',(#11378),#20073);
#11313=REPRESENTATION('density',(#11148),#20073);
#11314=REPRESENTATION('material name',(#11379),#20074);
#11315=REPRESENTATION('density',(#11149),#20074);
#11316=REPRESENTATION('material name',(#11380),#20075);
#11317=REPRESENTATION('density',(#11150),#20075);
#11318=REPRESENTATION('material name',(#11381),#20077);
#11319=REPRESENTATION('density',(#11151),#20077);
#11320=REPRESENTATION('material name',(#11382),#20078);
#11321=REPRESENTATION('density',(#11152),#20078);
#11322=REPRESENTATION('material name',(#11383),#20079);
#11323=REPRESENTATION('density',(#11153),#20079);
#11324=REPRESENTATION('material name',(#11384),#20080);
#11325=REPRESENTATION('density',(#11154),#20080);
#11326=REPRESENTATION('material name',(#11385),#20081);
#11327=REPRESENTATION('density',(#11155),#20081);
#11328=REPRESENTATION('material name',(#11386),#20082);
#11329=REPRESENTATION('density',(#11156),#20082);
#11330=REPRESENTATION('material name',(#11387),#20083);
#11331=REPRESENTATION('density',(#11157),#20083);
#11332=REPRESENTATION('material name',(#11388),#20085);
#11333=REPRESENTATION('density',(#11158),#20085);
#11334=REPRESENTATION('material name',(#11389),#20086);
#11335=REPRESENTATION('density',(#11159),#20086);
#11336=REPRESENTATION('material name',(#11390),#20087);
#11337=REPRESENTATION('density',(#11160),#20087);
#11338=REPRESENTATION('material name',(#11391),#20089);
#11339=REPRESENTATION('density',(#11161),#20089);
#11340=REPRESENTATION('material name',(#11392),#20090);
#11341=REPRESENTATION('density',(#11162),#20090);
#11342=REPRESENTATION('material name',(#11393),#20091);
#11343=REPRESENTATION('density',(#11163),#20091);
#11344=REPRESENTATION('material name',(#11394),#20092);
#11345=REPRESENTATION('density',(#11164),#20092);
#11346=REPRESENTATION('material name',(#11395),#20093);
#11347=REPRESENTATION('density',(#11165),#20093);
#11348=REPRESENTATION('material name',(#11396),#20094);
#11349=REPRESENTATION('density',(#11166),#20094);
#11350=REPRESENTATION('material name',(#11397),#20095);
#11351=REPRESENTATION('density',(#11167),#20095);
#11352=DESCRIPTIVE_REPRESENTATION_ITEM('Steel','Steel');
#11353=DESCRIPTIVE_REPRESENTATION_ITEM('Steel','Steel');
#11354=DESCRIPTIVE_REPRESENTATION_ITEM('Steel','Steel');
#11355=DESCRIPTIVE_REPRESENTATION_ITEM('Steel','Steel');
#11356=DESCRIPTIVE_REPRESENTATION_ITEM('Steel','Steel');
#11357=DESCRIPTIVE_REPRESENTATION_ITEM('Steel','Steel');
#11358=DESCRIPTIVE_REPRESENTATION_ITEM('Steel','Steel');
#11359=DESCRIPTIVE_REPRESENTATION_ITEM('Steel','Steel');
#11360=DESCRIPTIVE_REPRESENTATION_ITEM('Steel','Steel');
#11361=DESCRIPTIVE_REPRESENTATION_ITEM('Steel','Steel');
#11362=DESCRIPTIVE_REPRESENTATION_ITEM('Steel','Steel');
#11363=DESCRIPTIVE_REPRESENTATION_ITEM('Steel','Steel');
#11364=DESCRIPTIVE_REPRESENTATION_ITEM('Steel','Steel');
#11365=DESCRIPTIVE_REPRESENTATION_ITEM('Steel','Steel');
#11366=DESCRIPTIVE_REPRESENTATION_ITEM('Steel','Steel');
#11367=DESCRIPTIVE_REPRESENTATION_ITEM('Steel','Steel');
#11368=DESCRIPTIVE_REPRESENTATION_ITEM('Steel','Steel');
#11369=DESCRIPTIVE_REPRESENTATION_ITEM('Steel','Steel');
#11370=DESCRIPTIVE_REPRESENTATION_ITEM('Steel','Steel');
#11371=DESCRIPTIVE_REPRESENTATION_ITEM('Steel','Steel');
#11372=DESCRIPTIVE_REPRESENTATION_ITEM('Steel','Steel');
#11373=DESCRIPTIVE_REPRESENTATION_ITEM('Steel','Steel');
#11374=DESCRIPTIVE_REPRESENTATION_ITEM('Steel','Steel');
#11375=DESCRIPTIVE_REPRESENTATION_ITEM('Steel','Steel');
#11376=DESCRIPTIVE_REPRESENTATION_ITEM('Steel','Steel');
#11377=DESCRIPTIVE_REPRESENTATION_ITEM('Steel','Steel');
#11378=DESCRIPTIVE_REPRESENTATION_ITEM('Steel','Steel');
#11379=DESCRIPTIVE_REPRESENTATION_ITEM('Steel','Steel');
#11380=DESCRIPTIVE_REPRESENTATION_ITEM('Steel','Steel');
#11381=DESCRIPTIVE_REPRESENTATION_ITEM('Steel','Steel');
#11382=DESCRIPTIVE_REPRESENTATION_ITEM('Steel','Steel');
#11383=DESCRIPTIVE_REPRESENTATION_ITEM('Steel','Steel');
#11384=DESCRIPTIVE_REPRESENTATION_ITEM('Steel','Steel');
#11385=DESCRIPTIVE_REPRESENTATION_ITEM('Steel','Steel');
#11386=DESCRIPTIVE_REPRESENTATION_ITEM('Steel','Steel');
#11387=DESCRIPTIVE_REPRESENTATION_ITEM('Steel','Steel');
#11388=DESCRIPTIVE_REPRESENTATION_ITEM('Steel','Steel');
#11389=DESCRIPTIVE_REPRESENTATION_ITEM('Steel','Steel');
#11390=DESCRIPTIVE_REPRESENTATION_ITEM('Steel','Steel');
#11391=DESCRIPTIVE_REPRESENTATION_ITEM('Steel','Steel');
#11392=DESCRIPTIVE_REPRESENTATION_ITEM('Steel','Steel');
#11393=DESCRIPTIVE_REPRESENTATION_ITEM('Steel','Steel');
#11394=DESCRIPTIVE_REPRESENTATION_ITEM('Steel','Steel');
#11395=DESCRIPTIVE_REPRESENTATION_ITEM('Steel','Steel');
#11396=DESCRIPTIVE_REPRESENTATION_ITEM('Steel','Steel');
#11397=DESCRIPTIVE_REPRESENTATION_ITEM('Steel','Steel');
#11398=PROPERTY_DEFINITION('material property','material name',#20368);
#11399=PROPERTY_DEFINITION('material property','density of part',#20368);
#11400=PROPERTY_DEFINITION('material property','material name',#20369);
#11401=PROPERTY_DEFINITION('material property','density of part',#20369);
#11402=PROPERTY_DEFINITION('material property','material name',#20370);
#11403=PROPERTY_DEFINITION('material property','density of part',#20370);
#11404=PROPERTY_DEFINITION('material property','material name',#20371);
#11405=PROPERTY_DEFINITION('material property','density of part',#20371);
#11406=PROPERTY_DEFINITION('material property','material name',#20372);
#11407=PROPERTY_DEFINITION('material property','density of part',#20372);
#11408=PROPERTY_DEFINITION('material property','material name',#20373);
#11409=PROPERTY_DEFINITION('material property','density of part',#20373);
#11410=PROPERTY_DEFINITION('material property','material name',#20374);
#11411=PROPERTY_DEFINITION('material property','density of part',#20374);
#11412=PROPERTY_DEFINITION('material property','material name',#20375);
#11413=PROPERTY_DEFINITION('material property','density of part',#20375);
#11414=PROPERTY_DEFINITION('material property','material name',#20376);
#11415=PROPERTY_DEFINITION('material property','density of part',#20376);
#11416=PROPERTY_DEFINITION('material property','material name',#20377);
#11417=PROPERTY_DEFINITION('material property','density of part',#20377);
#11418=PROPERTY_DEFINITION('material property','material name',#20378);
#11419=PROPERTY_DEFINITION('material property','density of part',#20378);
#11420=PROPERTY_DEFINITION('material property','material name',#20379);
#11421=PROPERTY_DEFINITION('material property','density of part',#20379);
#11422=PROPERTY_DEFINITION('material property','material name',#20380);
#11423=PROPERTY_DEFINITION('material property','density of part',#20380);
#11424=PROPERTY_DEFINITION('material property','material name',#20381);
#11425=PROPERTY_DEFINITION('material property','density of part',#20381);
#11426=PROPERTY_DEFINITION('material property','material name',#20383);
#11427=PROPERTY_DEFINITION('material property','density of part',#20383);
#11428=PROPERTY_DEFINITION('material property','material name',#20384);
#11429=PROPERTY_DEFINITION('material property','density of part',#20384);
#11430=PROPERTY_DEFINITION('material property','material name',#20385);
#11431=PROPERTY_DEFINITION('material property','density of part',#20385);
#11432=PROPERTY_DEFINITION('material property','material name',#20386);
#11433=PROPERTY_DEFINITION('material property','density of part',#20386);
#11434=PROPERTY_DEFINITION('material property','material name',#20387);
#11435=PROPERTY_DEFINITION('material property','density of part',#20387);
#11436=PROPERTY_DEFINITION('material property','material name',#20388);
#11437=PROPERTY_DEFINITION('material property','density of part',#20388);
#11438=PROPERTY_DEFINITION('material property','material name',#20389);
#11439=PROPERTY_DEFINITION('material property','density of part',#20389);
#11440=PROPERTY_DEFINITION('material property','material name',#20390);
#11441=PROPERTY_DEFINITION('material property','density of part',#20390);
#11442=PROPERTY_DEFINITION('material property','material name',#20391);
#11443=PROPERTY_DEFINITION('material property','density of part',#20391);
#11444=PROPERTY_DEFINITION('material property','material name',#20393);
#11445=PROPERTY_DEFINITION('material property','density of part',#20393);
#11446=PROPERTY_DEFINITION('material property','material name',#20394);
#11447=PROPERTY_DEFINITION('material property','density of part',#20394);
#11448=PROPERTY_DEFINITION('material property','material name',#20395);
#11449=PROPERTY_DEFINITION('material property','density of part',#20395);
#11450=PROPERTY_DEFINITION('material property','material name',#20396);
#11451=PROPERTY_DEFINITION('material property','density of part',#20396);
#11452=PROPERTY_DEFINITION('material property','material name',#20397);
#11453=PROPERTY_DEFINITION('material property','density of part',#20397);
#11454=PROPERTY_DEFINITION('material property','material name',#20398);
#11455=PROPERTY_DEFINITION('material property','density of part',#20398);
#11456=PROPERTY_DEFINITION('material property','material name',#20400);
#11457=PROPERTY_DEFINITION('material property','density of part',#20400);
#11458=PROPERTY_DEFINITION('material property','material name',#20401);
#11459=PROPERTY_DEFINITION('material property','density of part',#20401);
#11460=PROPERTY_DEFINITION('material property','material name',#20402);
#11461=PROPERTY_DEFINITION('material property','density of part',#20402);
#11462=PROPERTY_DEFINITION('material property','material name',#20403);
#11463=PROPERTY_DEFINITION('material property','density of part',#20403);
#11464=PROPERTY_DEFINITION('material property','material name',#20404);
#11465=PROPERTY_DEFINITION('material property','density of part',#20404);
#11466=PROPERTY_DEFINITION('material property','material name',#20405);
#11467=PROPERTY_DEFINITION('material property','density of part',#20405);
#11468=PROPERTY_DEFINITION('material property','material name',#20406);
#11469=PROPERTY_DEFINITION('material property','density of part',#20406);
#11470=PROPERTY_DEFINITION('material property','material name',#20408);
#11471=PROPERTY_DEFINITION('material property','density of part',#20408);
#11472=PROPERTY_DEFINITION('material property','material name',#20409);
#11473=PROPERTY_DEFINITION('material property','density of part',#20409);
#11474=PROPERTY_DEFINITION('material property','material name',#20410);
#11475=PROPERTY_DEFINITION('material property','density of part',#20410);
#11476=PROPERTY_DEFINITION('material property','material name',#20412);
#11477=PROPERTY_DEFINITION('material property','density of part',#20412);
#11478=PROPERTY_DEFINITION('material property','material name',#20413);
#11479=PROPERTY_DEFINITION('material property','density of part',#20413);
#11480=PROPERTY_DEFINITION('material property','material name',#20414);
#11481=PROPERTY_DEFINITION('material property','density of part',#20414);
#11482=PROPERTY_DEFINITION('material property','material name',#20415);
#11483=PROPERTY_DEFINITION('material property','density of part',#20415);
#11484=PROPERTY_DEFINITION('material property','material name',#20416);
#11485=PROPERTY_DEFINITION('material property','density of part',#20416);
#11486=PROPERTY_DEFINITION('material property','material name',#20417);
#11487=PROPERTY_DEFINITION('material property','density of part',#20417);
#11488=PROPERTY_DEFINITION('material property','material name',#20418);
#11489=PROPERTY_DEFINITION('material property','density of part',#20418);
#11490=AXIS2_PLACEMENT_3D('',#16232,#12785,#12786);
#11491=AXIS2_PLACEMENT_3D('',#16233,#12787,#12788);
#11492=AXIS2_PLACEMENT_3D('',#16234,#12789,#12790);
#11493=AXIS2_PLACEMENT_3D('',#16235,#12791,#12792);
#11494=AXIS2_PLACEMENT_3D('',#16237,#12793,#12794);
#11495=AXIS2_PLACEMENT_3D('',#16240,#12796,#12797);
#11496=AXIS2_PLACEMENT_3D('',#16241,#12798,#12799);
#11497=AXIS2_PLACEMENT_3D('',#16242,#12800,#12801);
#11498=AXIS2_PLACEMENT_3D('',#16244,#12802,#12803);
#11499=AXIS2_PLACEMENT_3D('',#16247,#12805,#12806);
#11500=AXIS2_PLACEMENT_3D('',#16248,#12807,#12808);
#11501=AXIS2_PLACEMENT_3D('',#16249,#12809,#12810);
#11502=AXIS2_PLACEMENT_3D('',#16251,#12811,#12812);
#11503=AXIS2_PLACEMENT_3D('',#16254,#12814,#12815);
#11504=AXIS2_PLACEMENT_3D('',#16255,#12816,#12817);
#11505=AXIS2_PLACEMENT_3D('',#16256,#12818,#12819);
#11506=AXIS2_PLACEMENT_3D('',#16258,#12820,#12821);
#11507=AXIS2_PLACEMENT_3D('',#16261,#12823,#12824);
#11508=AXIS2_PLACEMENT_3D('',#16262,#12825,#12826);
#11509=AXIS2_PLACEMENT_3D('',#16263,#12827,#12828);
#11510=AXIS2_PLACEMENT_3D('',#16265,#12829,#12830);
#11511=AXIS2_PLACEMENT_3D('',#16268,#12832,#12833);
#11512=AXIS2_PLACEMENT_3D('',#16269,#12834,#12835);
#11513=AXIS2_PLACEMENT_3D('',#16270,#12836,#12837);
#11514=AXIS2_PLACEMENT_3D('',#16272,#12838,#12839);
#11515=AXIS2_PLACEMENT_3D('',#16275,#12841,#12842);
#11516=AXIS2_PLACEMENT_3D('',#16276,#12843,#12844);
#11517=AXIS2_PLACEMENT_3D('',#16277,#12845,#12846);
#11518=AXIS2_PLACEMENT_3D('',#16279,#12847,#12848);
#11519=AXIS2_PLACEMENT_3D('',#16282,#12850,#12851);
#11520=AXIS2_PLACEMENT_3D('',#16283,#12852,#12853);
#11521=AXIS2_PLACEMENT_3D('',#16284,#12854,#12855);
#11522=AXIS2_PLACEMENT_3D('',#16286,#12856,#12857);
#11523=AXIS2_PLACEMENT_3D('',#16289,#12859,#12860);
#11524=AXIS2_PLACEMENT_3D('',#16290,#12861,#12862);
#11525=AXIS2_PLACEMENT_3D('',#16291,#12863,#12864);
#11526=AXIS2_PLACEMENT_3D('',#16293,#12865,#12866);
#11527=AXIS2_PLACEMENT_3D('',#16296,#12868,#12869);
#11528=AXIS2_PLACEMENT_3D('',#16297,#12870,#12871);
#11529=AXIS2_PLACEMENT_3D('',#16299,#12872,#12873);
#11530=AXIS2_PLACEMENT_3D('',#16302,#12875,#12876);
#11531=AXIS2_PLACEMENT_3D('',#16303,#12877,#12878);
#11532=AXIS2_PLACEMENT_3D('',#16305,#12879,#12880);
#11533=AXIS2_PLACEMENT_3D('',#16308,#12882,#12883);
#11534=AXIS2_PLACEMENT_3D('',#16309,#12884,#12885);
#11535=AXIS2_PLACEMENT_3D('',#16311,#12886,#12887);
#11536=AXIS2_PLACEMENT_3D('',#16314,#12889,#12890);
#11537=AXIS2_PLACEMENT_3D('',#16315,#12891,#12892);
#11538=AXIS2_PLACEMENT_3D('',#16317,#12893,#12894);
#11539=AXIS2_PLACEMENT_3D('',#16320,#12896,#12897);
#11540=AXIS2_PLACEMENT_3D('',#16321,#12898,#12899);
#11541=AXIS2_PLACEMENT_3D('',#16322,#12900,#12901);
#11542=AXIS2_PLACEMENT_3D('',#16324,#12902,#12903);
#11543=AXIS2_PLACEMENT_3D('',#16327,#12905,#12906);
#11544=AXIS2_PLACEMENT_3D('',#16328,#12907,#12908);
#11545=AXIS2_PLACEMENT_3D('',#16329,#12909,#12910);
#11546=AXIS2_PLACEMENT_3D('',#16331,#12911,#12912);
#11547=AXIS2_PLACEMENT_3D('',#16334,#12914,#12915);
#11548=AXIS2_PLACEMENT_3D('',#16335,#12916,#12917);
#11549=AXIS2_PLACEMENT_3D('',#16336,#12918,#12919);
#11550=AXIS2_PLACEMENT_3D('',#16338,#12920,#12921);
#11551=AXIS2_PLACEMENT_3D('',#16341,#12923,#12924);
#11552=AXIS2_PLACEMENT_3D('',#16342,#12925,#12926);
#11553=AXIS2_PLACEMENT_3D('',#16343,#12927,#12928);
#11554=AXIS2_PLACEMENT_3D('',#16345,#12929,#12930);
#11555=AXIS2_PLACEMENT_3D('',#16348,#12932,#12933);
#11556=AXIS2_PLACEMENT_3D('',#16349,#12934,#12935);
#11557=AXIS2_PLACEMENT_3D('',#16350,#12936,#12937);
#11558=AXIS2_PLACEMENT_3D('',#16352,#12938,#12939);
#11559=AXIS2_PLACEMENT_3D('',#16355,#12941,#12942);
#11560=AXIS2_PLACEMENT_3D('',#16356,#12943,#12944);
#11561=AXIS2_PLACEMENT_3D('',#16357,#12945,#12946);
#11562=AXIS2_PLACEMENT_3D('',#16359,#12947,#12948);
#11563=AXIS2_PLACEMENT_3D('',#16362,#12950,#12951);
#11564=AXIS2_PLACEMENT_3D('',#16363,#12952,#12953);
#11565=AXIS2_PLACEMENT_3D('',#16364,#12954,#12955);
#11566=AXIS2_PLACEMENT_3D('',#16366,#12956,#12957);
#11567=AXIS2_PLACEMENT_3D('',#16369,#12959,#12960);
#11568=AXIS2_PLACEMENT_3D('',#16370,#12961,#12962);
#11569=AXIS2_PLACEMENT_3D('',#16371,#12963,#12964);
#11570=AXIS2_PLACEMENT_3D('',#16380,#12969,#12970);
#11571=AXIS2_PLACEMENT_3D('',#16386,#12974,#12975);
#11572=AXIS2_PLACEMENT_3D('',#16392,#12979,#12980);
#11573=AXIS2_PLACEMENT_3D('',#16395,#12983,#12984);
#11574=AXIS2_PLACEMENT_3D('',#16396,#12985,#12986);
#11575=AXIS2_PLACEMENT_3D('',#16397,#12987,#12988);
#11576=AXIS2_PLACEMENT_3D('',#16398,#12989,#12990);
#11577=AXIS2_PLACEMENT_3D('',#16407,#12995,#12996);
#11578=AXIS2_PLACEMENT_3D('',#16413,#13000,#13001);
#11579=AXIS2_PLACEMENT_3D('',#16417,#13004,#13005);
#11580=AXIS2_PLACEMENT_3D('',#16421,#13008,#13009);
#11581=AXIS2_PLACEMENT_3D('',#16423,#13011,#13012);
#11582=AXIS2_PLACEMENT_3D('',#16424,#13013,#13014);
#11583=AXIS2_PLACEMENT_3D('',#16433,#13019,#13020);
#11584=AXIS2_PLACEMENT_3D('',#16439,#13024,#13025);
#11585=AXIS2_PLACEMENT_3D('',#16443,#13028,#13029);
#11586=AXIS2_PLACEMENT_3D('',#16447,#13032,#13033);
#11587=AXIS2_PLACEMENT_3D('',#16449,#13035,#13036);
#11588=AXIS2_PLACEMENT_3D('',#16450,#13037,#13038);
#11589=AXIS2_PLACEMENT_3D('',#16451,#13039,#13040);
#11590=AXIS2_PLACEMENT_3D('',#16460,#13045,#13046);
#11591=AXIS2_PLACEMENT_3D('',#16466,#13050,#13051);
#11592=AXIS2_PLACEMENT_3D('',#16470,#13054,#13055);
#11593=AXIS2_PLACEMENT_3D('',#16474,#13058,#13059);
#11594=AXIS2_PLACEMENT_3D('',#16476,#13061,#13062);
#11595=AXIS2_PLACEMENT_3D('',#16477,#13063,#13064);
#11596=AXIS2_PLACEMENT_3D('',#16486,#13069,#13070);
#11597=AXIS2_PLACEMENT_3D('',#16492,#13074,#13075);
#11598=AXIS2_PLACEMENT_3D('',#16496,#13078,#13079);
#11599=AXIS2_PLACEMENT_3D('',#16500,#13082,#13083);
#11600=AXIS2_PLACEMENT_3D('',#16502,#13085,#13086);
#11601=AXIS2_PLACEMENT_3D('',#16503,#13087,#13088);
#11602=AXIS2_PLACEMENT_3D('',#16504,#13089,#13090);
#11603=AXIS2_PLACEMENT_3D('',#16506,#13091,#13092);
#11604=AXIS2_PLACEMENT_3D('',#16509,#13094,#13095);
#11605=AXIS2_PLACEMENT_3D('',#16510,#13096,#13097);
#11606=AXIS2_PLACEMENT_3D('',#16512,#13098,#13099);
#11607=AXIS2_PLACEMENT_3D('',#16515,#13101,#13102);
#11608=AXIS2_PLACEMENT_3D('',#16516,#13103,#13104);
#11609=AXIS2_PLACEMENT_3D('',#16518,#13105,#13106);
#11610=AXIS2_PLACEMENT_3D('',#16521,#13108,#13109);
#11611=AXIS2_PLACEMENT_3D('',#16522,#13110,#13111);
#11612=AXIS2_PLACEMENT_3D('',#16524,#13112,#13113);
#11613=AXIS2_PLACEMENT_3D('',#16527,#13115,#13116);
#11614=AXIS2_PLACEMENT_3D('',#16528,#13117,#13118);
#11615=AXIS2_PLACEMENT_3D('',#16530,#13119,#13120);
#11616=AXIS2_PLACEMENT_3D('',#16533,#13122,#13123);
#11617=AXIS2_PLACEMENT_3D('',#16534,#13124,#13125);
#11618=AXIS2_PLACEMENT_3D('',#16536,#13126,#13127);
#11619=AXIS2_PLACEMENT_3D('',#16539,#13129,#13130);
#11620=AXIS2_PLACEMENT_3D('',#16540,#13131,#13132);
#11621=AXIS2_PLACEMENT_3D('',#16542,#13133,#13134);
#11622=AXIS2_PLACEMENT_3D('',#16545,#13136,#13137);
#11623=AXIS2_PLACEMENT_3D('',#16546,#13138,#13139);
#11624=AXIS2_PLACEMENT_3D('',#16548,#13140,#13141);
#11625=AXIS2_PLACEMENT_3D('',#16551,#13143,#13144);
#11626=AXIS2_PLACEMENT_3D('',#16552,#13145,#13146);
#11627=AXIS2_PLACEMENT_3D('',#16554,#13147,#13148);
#11628=AXIS2_PLACEMENT_3D('',#16557,#13150,#13151);
#11629=AXIS2_PLACEMENT_3D('',#16558,#13152,#13153);
#11630=AXIS2_PLACEMENT_3D('',#16567,#13158,#13159);
#11631=AXIS2_PLACEMENT_3D('',#16576,#13164,#13165);
#11632=AXIS2_PLACEMENT_3D('',#16582,#13169,#13170);
#11633=AXIS2_PLACEMENT_3D('',#16588,#13174,#13175);
#11634=AXIS2_PLACEMENT_3D('',#16595,#13180,#13181);
#11635=AXIS2_PLACEMENT_3D('',#16599,#13184,#13185);
#11636=AXIS2_PLACEMENT_3D('',#16604,#13189,#13190);
#11637=AXIS2_PLACEMENT_3D('',#16606,#13192,#13193);
#11638=AXIS2_PLACEMENT_3D('',#16607,#13194,#13195);
#11639=AXIS2_PLACEMENT_3D('',#16608,#13196,#13197);
#11640=AXIS2_PLACEMENT_3D('',#16609,#13198,#13199);
#11641=AXIS2_PLACEMENT_3D('',#16611,#13200,#13201);
#11642=AXIS2_PLACEMENT_3D('',#16614,#13203,#13204);
#11643=AXIS2_PLACEMENT_3D('',#16615,#13205,#13206);
#11644=AXIS2_PLACEMENT_3D('',#16617,#13207,#13208);
#11645=AXIS2_PLACEMENT_3D('',#16620,#13210,#13211);
#11646=AXIS2_PLACEMENT_3D('',#16621,#13212,#13213);
#11647=AXIS2_PLACEMENT_3D('',#16622,#13214,#13215);
#11648=AXIS2_PLACEMENT_3D('',#16623,#13216,#13217);
#11649=AXIS2_PLACEMENT_3D('',#16624,#13218,#13219);
#11650=AXIS2_PLACEMENT_3D('',#16629,#13221,#13222);
#11651=AXIS2_PLACEMENT_3D('',#16632,#13224,#13225);
#11652=AXIS2_PLACEMENT_3D('',#16633,#13226,#13227);
#11653=AXIS2_PLACEMENT_3D('',#16638,#13229,#13230);
#11654=AXIS2_PLACEMENT_3D('',#16641,#13232,#13233);
#11655=AXIS2_PLACEMENT_3D('',#16642,#13234,#13235);
#11656=AXIS2_PLACEMENT_3D('',#16647,#13237,#13238);
#11657=AXIS2_PLACEMENT_3D('',#16650,#13240,#13241);
#11658=AXIS2_PLACEMENT_3D('',#16651,#13242,#13243);
#11659=AXIS2_PLACEMENT_3D('',#16656,#13245,#13246);
#11660=AXIS2_PLACEMENT_3D('',#16659,#13248,#13249);
#11661=AXIS2_PLACEMENT_3D('',#16660,#13250,#13251);
#11662=AXIS2_PLACEMENT_3D('',#16661,#13252,#13253);
#11663=AXIS2_PLACEMENT_3D('',#16662,#13254,#13255);
#11664=AXIS2_PLACEMENT_3D('',#16663,#13256,#13257);
#11665=AXIS2_PLACEMENT_3D('',#16664,#13258,#13259);
#11666=AXIS2_PLACEMENT_3D('',#16666,#13260,#13261);
#11667=AXIS2_PLACEMENT_3D('',#16667,#13262,#13263);
#11668=AXIS2_PLACEMENT_3D('',#16668,#13264,#13265);
#11669=AXIS2_PLACEMENT_3D('',#16669,#13266,#13267);
#11670=AXIS2_PLACEMENT_3D('',#16670,#13268,#13269);
#11671=AXIS2_PLACEMENT_3D('',#16671,#13270,#13271);
#11672=AXIS2_PLACEMENT_3D('',#16672,#13272,#13273);
#11673=AXIS2_PLACEMENT_3D('',#16673,#13274,#13275);
#11674=AXIS2_PLACEMENT_3D('',#16674,#13276,#13277);
#11675=AXIS2_PLACEMENT_3D('',#16675,#13278,#13279);
#11676=AXIS2_PLACEMENT_3D('',#16677,#13280,#13281);
#11677=AXIS2_PLACEMENT_3D('',#16680,#13283,#13284);
#11678=AXIS2_PLACEMENT_3D('',#16681,#13285,#13286);
#11679=AXIS2_PLACEMENT_3D('',#16683,#13287,#13288);
#11680=AXIS2_PLACEMENT_3D('',#16684,#13289,#13290);
#11681=AXIS2_PLACEMENT_3D('',#16686,#13292,#13293);
#11682=AXIS2_PLACEMENT_3D('',#16687,#13294,#13295);
#11683=AXIS2_PLACEMENT_3D('',#16688,#13296,#13297);
#11684=AXIS2_PLACEMENT_3D('',#16693,#13299,#13300);
#11685=AXIS2_PLACEMENT_3D('',#16696,#13302,#13303);
#11686=AXIS2_PLACEMENT_3D('',#16697,#13304,#13305);
#11687=AXIS2_PLACEMENT_3D('',#16702,#13307,#13308);
#11688=AXIS2_PLACEMENT_3D('',#16705,#13310,#13311);
#11689=AXIS2_PLACEMENT_3D('',#16706,#13312,#13313);
#11690=AXIS2_PLACEMENT_3D('',#16711,#13315,#13316);
#11691=AXIS2_PLACEMENT_3D('',#16714,#13318,#13319);
#11692=AXIS2_PLACEMENT_3D('',#16715,#13320,#13321);
#11693=AXIS2_PLACEMENT_3D('',#16720,#13323,#13324);
#11694=AXIS2_PLACEMENT_3D('',#16723,#13326,#13327);
#11695=AXIS2_PLACEMENT_3D('',#16724,#13328,#13329);
#11696=AXIS2_PLACEMENT_3D('',#16725,#13330,#13331);
#11697=AXIS2_PLACEMENT_3D('',#16726,#13332,#13333);
#11698=AXIS2_PLACEMENT_3D('',#16727,#13334,#13335);
#11699=AXIS2_PLACEMENT_3D('',#16728,#13336,#13337);
#11700=AXIS2_PLACEMENT_3D('',#16730,#13338,#13339);
#11701=AXIS2_PLACEMENT_3D('',#16731,#13340,#13341);
#11702=AXIS2_PLACEMENT_3D('',#16732,#13342,#13343);
#11703=AXIS2_PLACEMENT_3D('',#16733,#13344,#13345);
#11704=AXIS2_PLACEMENT_3D('',#16734,#13346,#13347);
#11705=AXIS2_PLACEMENT_3D('',#16735,#13348,#13349);
#11706=AXIS2_PLACEMENT_3D('',#16736,#13350,#13351);
#11707=AXIS2_PLACEMENT_3D('',#16737,#13352,#13353);
#11708=AXIS2_PLACEMENT_3D('',#16738,#13354,#13355);
#11709=AXIS2_PLACEMENT_3D('',#16739,#13356,#13357);
#11710=AXIS2_PLACEMENT_3D('',#16742,#13359,#13360);
#11711=AXIS2_PLACEMENT_3D('',#16743,#13361,#13362);
#11712=AXIS2_PLACEMENT_3D('',#16745,#13363,#13364);
#11713=AXIS2_PLACEMENT_3D('',#16746,#13365,#13366);
#11714=AXIS2_PLACEMENT_3D('',#16748,#13367,#13368);
#11715=AXIS2_PLACEMENT_3D('',#16750,#13370,#13371);
#11716=AXIS2_PLACEMENT_3D('',#16751,#13372,#13373);
#11717=AXIS2_PLACEMENT_3D('',#16752,#13374,#13375);
#11718=AXIS2_PLACEMENT_3D('',#16754,#13376,#13377);
#11719=AXIS2_PLACEMENT_3D('',#16757,#13379,#13380);
#11720=AXIS2_PLACEMENT_3D('',#16758,#13381,#13382);
#11721=AXIS2_PLACEMENT_3D('',#16760,#13383,#13384);
#11722=AXIS2_PLACEMENT_3D('',#16763,#13386,#13387);
#11723=AXIS2_PLACEMENT_3D('',#16764,#13388,#13389);
#11724=AXIS2_PLACEMENT_3D('',#16766,#13390,#13391);
#11725=AXIS2_PLACEMENT_3D('',#16769,#13393,#13394);
#11726=AXIS2_PLACEMENT_3D('',#16770,#13395,#13396);
#11727=AXIS2_PLACEMENT_3D('',#16772,#13397,#13398);
#11728=AXIS2_PLACEMENT_3D('',#16775,#13400,#13401);
#11729=AXIS2_PLACEMENT_3D('',#16776,#13402,#13403);
#11730=AXIS2_PLACEMENT_3D('',#16778,#13404,#13405);
#11731=AXIS2_PLACEMENT_3D('',#16781,#13407,#13408);
#11732=AXIS2_PLACEMENT_3D('',#16782,#13409,#13410);
#11733=AXIS2_PLACEMENT_3D('',#16784,#13411,#13412);
#11734=AXIS2_PLACEMENT_3D('',#16787,#13414,#13415);
#11735=AXIS2_PLACEMENT_3D('',#16788,#13416,#13417);
#11736=AXIS2_PLACEMENT_3D('',#16790,#13418,#13419);
#11737=AXIS2_PLACEMENT_3D('',#16793,#13421,#13422);
#11738=AXIS2_PLACEMENT_3D('',#16794,#13423,#13424);
#11739=AXIS2_PLACEMENT_3D('',#16796,#13425,#13426);
#11740=AXIS2_PLACEMENT_3D('',#16799,#13428,#13429);
#11741=AXIS2_PLACEMENT_3D('',#16800,#13430,#13431);
#11742=AXIS2_PLACEMENT_3D('',#16802,#13432,#13433);
#11743=AXIS2_PLACEMENT_3D('',#16805,#13435,#13436);
#11744=AXIS2_PLACEMENT_3D('',#16806,#13437,#13438);
#11745=AXIS2_PLACEMENT_3D('',#16815,#13443,#13444);
#11746=AXIS2_PLACEMENT_3D('',#16824,#13449,#13450);
#11747=AXIS2_PLACEMENT_3D('',#16830,#13454,#13455);
#11748=AXIS2_PLACEMENT_3D('',#16836,#13459,#13460);
#11749=AXIS2_PLACEMENT_3D('',#16843,#13465,#13466);
#11750=AXIS2_PLACEMENT_3D('',#16847,#13469,#13470);
#11751=AXIS2_PLACEMENT_3D('',#16852,#13474,#13475);
#11752=AXIS2_PLACEMENT_3D('',#16854,#13477,#13478);
#11753=AXIS2_PLACEMENT_3D('',#16855,#13479,#13480);
#11754=AXIS2_PLACEMENT_3D('',#16856,#13481,#13482);
#11755=AXIS2_PLACEMENT_3D('',#16857,#13483,#13484);
#11756=AXIS2_PLACEMENT_3D('',#16859,#13485,#13486);
#11757=AXIS2_PLACEMENT_3D('',#16862,#13488,#13489);
#11758=AXIS2_PLACEMENT_3D('',#16863,#13490,#13491);
#11759=AXIS2_PLACEMENT_3D('',#16865,#13492,#13493);
#11760=AXIS2_PLACEMENT_3D('',#16868,#13495,#13496);
#11761=AXIS2_PLACEMENT_3D('',#16869,#13497,#13498);
#11762=AXIS2_PLACEMENT_3D('',#16870,#13499,#13500);
#11763=AXIS2_PLACEMENT_3D('',#16871,#13501,#13502);
#11764=AXIS2_PLACEMENT_3D('',#16872,#13503,#13504);
#11765=AXIS2_PLACEMENT_3D('',#16877,#13506,#13507);
#11766=AXIS2_PLACEMENT_3D('',#16880,#13509,#13510);
#11767=AXIS2_PLACEMENT_3D('',#16881,#13511,#13512);
#11768=AXIS2_PLACEMENT_3D('',#16886,#13514,#13515);
#11769=AXIS2_PLACEMENT_3D('',#16889,#13517,#13518);
#11770=AXIS2_PLACEMENT_3D('',#16890,#13519,#13520);
#11771=AXIS2_PLACEMENT_3D('',#16895,#13522,#13523);
#11772=AXIS2_PLACEMENT_3D('',#16898,#13525,#13526);
#11773=AXIS2_PLACEMENT_3D('',#16899,#13527,#13528);
#11774=AXIS2_PLACEMENT_3D('',#16904,#13530,#13531);
#11775=AXIS2_PLACEMENT_3D('',#16907,#13533,#13534);
#11776=AXIS2_PLACEMENT_3D('',#16908,#13535,#13536);
#11777=AXIS2_PLACEMENT_3D('',#16909,#13537,#13538);
#11778=AXIS2_PLACEMENT_3D('',#16910,#13539,#13540);
#11779=AXIS2_PLACEMENT_3D('',#16911,#13541,#13542);
#11780=AXIS2_PLACEMENT_3D('',#16912,#13543,#13544);
#11781=AXIS2_PLACEMENT_3D('',#16914,#13545,#13546);
#11782=AXIS2_PLACEMENT_3D('',#16915,#13547,#13548);
#11783=AXIS2_PLACEMENT_3D('',#16916,#13549,#13550);
#11784=AXIS2_PLACEMENT_3D('',#16917,#13551,#13552);
#11785=AXIS2_PLACEMENT_3D('',#16918,#13553,#13554);
#11786=AXIS2_PLACEMENT_3D('',#16919,#13555,#13556);
#11787=AXIS2_PLACEMENT_3D('',#16920,#13557,#13558);
#11788=AXIS2_PLACEMENT_3D('',#16921,#13559,#13560);
#11789=AXIS2_PLACEMENT_3D('',#16922,#13561,#13562);
#11790=AXIS2_PLACEMENT_3D('',#16923,#13563,#13564);
#11791=AXIS2_PLACEMENT_3D('',#16925,#13565,#13566);
#11792=AXIS2_PLACEMENT_3D('',#16928,#13568,#13569);
#11793=AXIS2_PLACEMENT_3D('',#16929,#13570,#13571);
#11794=AXIS2_PLACEMENT_3D('',#16931,#13572,#13573);
#11795=AXIS2_PLACEMENT_3D('',#16932,#13574,#13575);
#11796=AXIS2_PLACEMENT_3D('',#16934,#13577,#13578);
#11797=AXIS2_PLACEMENT_3D('',#16935,#13579,#13580);
#11798=AXIS2_PLACEMENT_3D('',#16936,#13581,#13582);
#11799=AXIS2_PLACEMENT_3D('',#16941,#13584,#13585);
#11800=AXIS2_PLACEMENT_3D('',#16944,#13587,#13588);
#11801=AXIS2_PLACEMENT_3D('',#16945,#13589,#13590);
#11802=AXIS2_PLACEMENT_3D('',#16950,#13592,#13593);
#11803=AXIS2_PLACEMENT_3D('',#16953,#13595,#13596);
#11804=AXIS2_PLACEMENT_3D('',#16954,#13597,#13598);
#11805=AXIS2_PLACEMENT_3D('',#16959,#13600,#13601);
#11806=AXIS2_PLACEMENT_3D('',#16962,#13603,#13604);
#11807=AXIS2_PLACEMENT_3D('',#16963,#13605,#13606);
#11808=AXIS2_PLACEMENT_3D('',#16968,#13608,#13609);
#11809=AXIS2_PLACEMENT_3D('',#16971,#13611,#13612);
#11810=AXIS2_PLACEMENT_3D('',#16972,#13613,#13614);
#11811=AXIS2_PLACEMENT_3D('',#16973,#13615,#13616);
#11812=AXIS2_PLACEMENT_3D('',#16974,#13617,#13618);
#11813=AXIS2_PLACEMENT_3D('',#16975,#13619,#13620);
#11814=AXIS2_PLACEMENT_3D('',#16976,#13621,#13622);
#11815=AXIS2_PLACEMENT_3D('',#16978,#13623,#13624);
#11816=AXIS2_PLACEMENT_3D('',#16979,#13625,#13626);
#11817=AXIS2_PLACEMENT_3D('',#16980,#13627,#13628);
#11818=AXIS2_PLACEMENT_3D('',#16981,#13629,#13630);
#11819=AXIS2_PLACEMENT_3D('',#16982,#13631,#13632);
#11820=AXIS2_PLACEMENT_3D('',#16983,#13633,#13634);
#11821=AXIS2_PLACEMENT_3D('',#16984,#13635,#13636);
#11822=AXIS2_PLACEMENT_3D('',#16985,#13637,#13638);
#11823=AXIS2_PLACEMENT_3D('',#16986,#13639,#13640);
#11824=AXIS2_PLACEMENT_3D('',#16987,#13641,#13642);
#11825=AXIS2_PLACEMENT_3D('',#16990,#13644,#13645);
#11826=AXIS2_PLACEMENT_3D('',#16991,#13646,#13647);
#11827=AXIS2_PLACEMENT_3D('',#16993,#13648,#13649);
#11828=AXIS2_PLACEMENT_3D('',#16994,#13650,#13651);
#11829=AXIS2_PLACEMENT_3D('',#16996,#13652,#13653);
#11830=AXIS2_PLACEMENT_3D('',#16998,#13655,#13656);
#11831=AXIS2_PLACEMENT_3D('',#16999,#13657,#13658);
#11832=AXIS2_PLACEMENT_3D('',#17000,#13659,#13660);
#11833=AXIS2_PLACEMENT_3D('',#17009,#13665,#13666);
#11834=AXIS2_PLACEMENT_3D('',#17018,#13671,#13672);
#11835=AXIS2_PLACEMENT_3D('',#17023,#13674,#13675);
#11836=AXIS2_PLACEMENT_3D('',#17026,#13677,#13678);
#11837=AXIS2_PLACEMENT_3D('',#17027,#13679,#13680);
#11838=AXIS2_PLACEMENT_3D('',#17028,#13681,#13682);
#11839=AXIS2_PLACEMENT_3D('',#17029,#13683,#13684);
#11840=AXIS2_PLACEMENT_3D('',#17030,#13685,#13686);
#11841=AXIS2_PLACEMENT_3D('',#17031,#13687,#13688);
#11842=AXIS2_PLACEMENT_3D('',#17032,#13689,#13690);
#11843=AXIS2_PLACEMENT_3D('',#17033,#13691,#13692);
#11844=AXIS2_PLACEMENT_3D('',#17037,#13694,#13695);
#11845=AXIS2_PLACEMENT_3D('',#17039,#13697,#13698);
#11846=AXIS2_PLACEMENT_3D('',#17043,#13701,#13702);
#11847=AXIS2_PLACEMENT_3D('',#17047,#13705,#13706);
#11848=AXIS2_PLACEMENT_3D('',#17048,#13707,#13708);
#11849=AXIS2_PLACEMENT_3D('',#17049,#13709,#13710);
#11850=AXIS2_PLACEMENT_3D('',#17050,#13711,#13712);
#11851=AXIS2_PLACEMENT_3D('',#17051,#13713,#13714);
#11852=AXIS2_PLACEMENT_3D('',#17056,#13716,#13717);
#11853=AXIS2_PLACEMENT_3D('',#17059,#13719,#13720);
#11854=AXIS2_PLACEMENT_3D('',#17060,#13721,#13722);
#11855=AXIS2_PLACEMENT_3D('',#17065,#13724,#13725);
#11856=AXIS2_PLACEMENT_3D('',#17068,#13727,#13728);
#11857=AXIS2_PLACEMENT_3D('',#17069,#13729,#13730);
#11858=AXIS2_PLACEMENT_3D('',#17073,#13733,#13734);
#11859=AXIS2_PLACEMENT_3D('',#17074,#13735,#13736);
#11860=AXIS2_PLACEMENT_3D('',#17079,#13738,#13739);
#11861=AXIS2_PLACEMENT_3D('',#17082,#13741,#13742);
#11862=AXIS2_PLACEMENT_3D('',#17083,#13743,#13744);
#11863=AXIS2_PLACEMENT_3D('',#17088,#13746,#13747);
#11864=AXIS2_PLACEMENT_3D('',#17091,#13749,#13750);
#11865=AXIS2_PLACEMENT_3D('',#17092,#13751,#13752);
#11866=AXIS2_PLACEMENT_3D('',#17096,#13755,#13756);
#11867=AXIS2_PLACEMENT_3D('',#17097,#13757,#13758);
#11868=AXIS2_PLACEMENT_3D('',#17116,#13769,#13770);
#11869=AXIS2_PLACEMENT_3D('',#17120,#13773,#13774);
#11870=AXIS2_PLACEMENT_3D('',#17124,#13777,#13778);
#11871=AXIS2_PLACEMENT_3D('',#17126,#13780,#13781);
#11872=AXIS2_PLACEMENT_3D('',#17128,#13782,#13783);
#11873=AXIS2_PLACEMENT_3D('',#17130,#13785,#13786);
#11874=AXIS2_PLACEMENT_3D('',#17132,#13787,#13788);
#11875=AXIS2_PLACEMENT_3D('',#17134,#13790,#13791);
#11876=AXIS2_PLACEMENT_3D('',#17140,#13795,#13796);
#11877=AXIS2_PLACEMENT_3D('',#17146,#13800,#13801);
#11878=AXIS2_PLACEMENT_3D('',#17148,#13803,#13804);
#11879=AXIS2_PLACEMENT_3D('',#17155,#13809,#13810);
#11880=AXIS2_PLACEMENT_3D('',#17157,#13812,#13813);
#11881=AXIS2_PLACEMENT_3D('',#17159,#13815,#13816);
#11882=AXIS2_PLACEMENT_3D('',#17160,#13817,#13818);
#11883=AXIS2_PLACEMENT_3D('',#17161,#13819,#13820);
#11884=AXIS2_PLACEMENT_3D('',#17162,#13821,#13822);
#11885=AXIS2_PLACEMENT_3D('',#17167,#13824,#13825);
#11886=AXIS2_PLACEMENT_3D('',#17170,#13827,#13828);
#11887=AXIS2_PLACEMENT_3D('',#17171,#13829,#13830);
#11888=AXIS2_PLACEMENT_3D('',#17176,#13832,#13833);
#11889=AXIS2_PLACEMENT_3D('',#17179,#13835,#13836);
#11890=AXIS2_PLACEMENT_3D('',#17180,#13837,#13838);
#11891=AXIS2_PLACEMENT_3D('',#17184,#13841,#13842);
#11892=AXIS2_PLACEMENT_3D('',#17185,#13843,#13844);
#11893=AXIS2_PLACEMENT_3D('',#17190,#13846,#13847);
#11894=AXIS2_PLACEMENT_3D('',#17193,#13849,#13850);
#11895=AXIS2_PLACEMENT_3D('',#17194,#13851,#13852);
#11896=AXIS2_PLACEMENT_3D('',#17199,#13854,#13855);
#11897=AXIS2_PLACEMENT_3D('',#17202,#13857,#13858);
#11898=AXIS2_PLACEMENT_3D('',#17203,#13859,#13860);
#11899=AXIS2_PLACEMENT_3D('',#17207,#13863,#13864);
#11900=AXIS2_PLACEMENT_3D('',#17208,#13865,#13866);
#11901=AXIS2_PLACEMENT_3D('',#17227,#13877,#13878);
#11902=AXIS2_PLACEMENT_3D('',#17231,#13881,#13882);
#11903=AXIS2_PLACEMENT_3D('',#17235,#13885,#13886);
#11904=AXIS2_PLACEMENT_3D('',#17237,#13888,#13889);
#11905=AXIS2_PLACEMENT_3D('',#17239,#13890,#13891);
#11906=AXIS2_PLACEMENT_3D('',#17241,#13893,#13894);
#11907=AXIS2_PLACEMENT_3D('',#17243,#13895,#13896);
#11908=AXIS2_PLACEMENT_3D('',#17245,#13898,#13899);
#11909=AXIS2_PLACEMENT_3D('',#17251,#13903,#13904);
#11910=AXIS2_PLACEMENT_3D('',#17257,#13908,#13909);
#11911=AXIS2_PLACEMENT_3D('',#17259,#13911,#13912);
#11912=AXIS2_PLACEMENT_3D('',#17266,#13917,#13918);
#11913=AXIS2_PLACEMENT_3D('',#17268,#13920,#13921);
#11914=AXIS2_PLACEMENT_3D('',#17270,#13923,#13924);
#11915=AXIS2_PLACEMENT_3D('',#17271,#13925,#13926);
#11916=AXIS2_PLACEMENT_3D('',#17272,#13927,#13928);
#11917=AXIS2_PLACEMENT_3D('',#17273,#13929,#13930);
#11918=AXIS2_PLACEMENT_3D('',#17274,#13931,#13932);
#11919=AXIS2_PLACEMENT_3D('',#17277,#13933,#13934);
#11920=AXIS2_PLACEMENT_3D('',#17278,#13935,#13936);
#11921=AXIS2_PLACEMENT_3D('',#17280,#13937,#13938);
#11922=AXIS2_PLACEMENT_3D('',#17282,#13939,#13940);
#11923=AXIS2_PLACEMENT_3D('',#17283,#13941,#13942);
#11924=AXIS2_PLACEMENT_3D('',#17284,#13943,#13944);
#11925=AXIS2_PLACEMENT_3D('',#17287,#13946,#13947);
#11926=AXIS2_PLACEMENT_3D('',#17288,#13948,#13949);
#11927=AXIS2_PLACEMENT_3D('',#17290,#13950,#13951);
#11928=AXIS2_PLACEMENT_3D('',#17293,#13953,#13954);
#11929=AXIS2_PLACEMENT_3D('',#17294,#13955,#13956);
#11930=AXIS2_PLACEMENT_3D('',#17297,#13958,#13959);
#11931=AXIS2_PLACEMENT_3D('',#17298,#13960,#13961);
#11932=AXIS2_PLACEMENT_3D('',#17299,#13962,#13963);
#11933=AXIS2_PLACEMENT_3D('',#17301,#13964,#13965);
#11934=AXIS2_PLACEMENT_3D('',#17303,#13967,#13968);
#11935=AXIS2_PLACEMENT_3D('',#17305,#13969,#13970);
#11936=AXIS2_PLACEMENT_3D('',#17306,#13971,#13972);
#11937=AXIS2_PLACEMENT_3D('',#17308,#13974,#13975);
#11938=AXIS2_PLACEMENT_3D('',#17309,#13976,#13977);
#11939=AXIS2_PLACEMENT_3D('',#17312,#13978,#13979);
#11940=AXIS2_PLACEMENT_3D('',#17313,#13980,#13981);
#11941=AXIS2_PLACEMENT_3D('',#17315,#13982,#13983);
#11942=AXIS2_PLACEMENT_3D('',#17317,#13984,#13985);
#11943=AXIS2_PLACEMENT_3D('',#17318,#13986,#13987);
#11944=AXIS2_PLACEMENT_3D('',#17319,#13988,#13989);
#11945=AXIS2_PLACEMENT_3D('',#17321,#13990,#13991);
#11946=AXIS2_PLACEMENT_3D('',#17323,#13993,#13994);
#11947=AXIS2_PLACEMENT_3D('',#17325,#13995,#13996);
#11948=AXIS2_PLACEMENT_3D('',#17327,#13997,#13998);
#11949=AXIS2_PLACEMENT_3D('',#17328,#13999,#14000);
#11950=AXIS2_PLACEMENT_3D('',#17330,#14001,#14002);
#11951=AXIS2_PLACEMENT_3D('',#17332,#14004,#14005);
#11952=AXIS2_PLACEMENT_3D('',#17334,#14006,#14007);
#11953=AXIS2_PLACEMENT_3D('',#17336,#14009,#14010);
#11954=AXIS2_PLACEMENT_3D('',#17338,#14011,#14012);
#11955=AXIS2_PLACEMENT_3D('',#17340,#14014,#14015);
#11956=AXIS2_PLACEMENT_3D('',#17341,#14016,#14017);
#11957=AXIS2_PLACEMENT_3D('',#17343,#14019,#14020);
#11958=AXIS2_PLACEMENT_3D('',#17344,#14021,#14022);
#11959=AXIS2_PLACEMENT_3D('',#17347,#14023,#14024);
#11960=AXIS2_PLACEMENT_3D('',#17348,#14025,#14026);
#11961=AXIS2_PLACEMENT_3D('',#17351,#14027,#14028);
#11962=AXIS2_PLACEMENT_3D('',#17352,#14029,#14030);
#11963=AXIS2_PLACEMENT_3D('',#17355,#14031,#14032);
#11964=AXIS2_PLACEMENT_3D('',#17356,#14033,#14034);
#11965=AXIS2_PLACEMENT_3D('',#17359,#14035,#14036);
#11966=AXIS2_PLACEMENT_3D('',#17360,#14037,#14038);
#11967=AXIS2_PLACEMENT_3D('',#17363,#14039,#14040);
#11968=AXIS2_PLACEMENT_3D('',#17364,#14041,#14042);
#11969=AXIS2_PLACEMENT_3D('',#17367,#14043,#14044);
#11970=AXIS2_PLACEMENT_3D('',#17368,#14045,#14046);
#11971=AXIS2_PLACEMENT_3D('',#17371,#14047,#14048);
#11972=AXIS2_PLACEMENT_3D('',#17372,#14049,#14050);
#11973=AXIS2_PLACEMENT_3D('',#17375,#14051,#14052);
#11974=AXIS2_PLACEMENT_3D('',#17376,#14053,#14054);
#11975=AXIS2_PLACEMENT_3D('',#17377,#14055,#14056);
#11976=AXIS2_PLACEMENT_3D('',#17403,#14057,#14058);
#11977=AXIS2_PLACEMENT_3D('',#17427,#14059,#14060);
#11978=AXIS2_PLACEMENT_3D('',#17428,#14061,#14062);
#11979=AXIS2_PLACEMENT_3D('',#17430,#14063,#14064);
#11980=AXIS2_PLACEMENT_3D('',#17455,#14065,#14066);
#11981=AXIS2_PLACEMENT_3D('',#17480,#14067,#14068);
#11982=AXIS2_PLACEMENT_3D('',#17496,#14070,#14071);
#11983=AXIS2_PLACEMENT_3D('',#17511,#14072,#14073);
#11984=AXIS2_PLACEMENT_3D('',#17536,#14074,#14075);
#11985=AXIS2_PLACEMENT_3D('',#17561,#14076,#14077);
#11986=AXIS2_PLACEMENT_3D('',#17586,#14078,#14079);
#11987=AXIS2_PLACEMENT_3D('',#17610,#14080,#14081);
#11988=AXIS2_PLACEMENT_3D('',#17611,#14082,#14083);
#11989=AXIS2_PLACEMENT_3D('',#17613,#14084,#14085);
#11990=AXIS2_PLACEMENT_3D('',#17614,#14086,#14087);
#11991=AXIS2_PLACEMENT_3D('',#17615,#14088,#14089);
#11992=AXIS2_PLACEMENT_3D('',#17639,#14090,#14091);
#11993=AXIS2_PLACEMENT_3D('',#17640,#14092,#14093);
#11994=AXIS2_PLACEMENT_3D('',#17642,#14094,#14095);
#11995=AXIS2_PLACEMENT_3D('',#17643,#14096,#14097);
#11996=AXIS2_PLACEMENT_3D('',#17644,#14098,#14099);
#11997=AXIS2_PLACEMENT_3D('',#17668,#14100,#14101);
#11998=AXIS2_PLACEMENT_3D('',#17669,#14102,#14103);
#11999=AXIS2_PLACEMENT_3D('',#17671,#14104,#14105);
#12000=AXIS2_PLACEMENT_3D('',#17672,#14106,#14107);
#12001=AXIS2_PLACEMENT_3D('',#17673,#14108,#14109);
#12002=AXIS2_PLACEMENT_3D('',#17688,#14110,#14111);
#12003=AXIS2_PLACEMENT_3D('',#17701,#14112,#14113);
#12004=AXIS2_PLACEMENT_3D('',#17703,#14114,#14115);
#12005=AXIS2_PLACEMENT_3D('',#17704,#14116,#14117);
#12006=AXIS2_PLACEMENT_3D('',#17705,#14118,#14119);
#12007=AXIS2_PLACEMENT_3D('',#17729,#14120,#14121);
#12008=AXIS2_PLACEMENT_3D('',#17730,#14122,#14123);
#12009=AXIS2_PLACEMENT_3D('',#17732,#14124,#14125);
#12010=AXIS2_PLACEMENT_3D('',#17733,#14126,#14127);
#12011=AXIS2_PLACEMENT_3D('',#17734,#14128,#14129);
#12012=AXIS2_PLACEMENT_3D('',#17758,#14130,#14131);
#12013=AXIS2_PLACEMENT_3D('',#17759,#14132,#14133);
#12014=AXIS2_PLACEMENT_3D('',#17761,#14134,#14135);
#12015=AXIS2_PLACEMENT_3D('',#17762,#14136,#14137);
#12016=AXIS2_PLACEMENT_3D('',#17763,#14138,#14139);
#12017=AXIS2_PLACEMENT_3D('',#17787,#14140,#14141);
#12018=AXIS2_PLACEMENT_3D('',#17788,#14142,#14143);
#12019=AXIS2_PLACEMENT_3D('',#17790,#14144,#14145);
#12020=AXIS2_PLACEMENT_3D('',#17793,#14147,#14148);
#12021=AXIS2_PLACEMENT_3D('',#17817,#14149,#14150);
#12022=AXIS2_PLACEMENT_3D('',#17818,#14151,#14152);
#12023=AXIS2_PLACEMENT_3D('',#17819,#14153,#14154);
#12024=AXIS2_PLACEMENT_3D('',#17820,#14155,#14156);
#12025=AXIS2_PLACEMENT_3D('',#17821,#14157,#14158);
#12026=AXIS2_PLACEMENT_3D('',#17822,#14159,#14160);
#12027=AXIS2_PLACEMENT_3D('',#17823,#14161,#14162);
#12028=AXIS2_PLACEMENT_3D('',#17824,#14163,#14164);
#12029=AXIS2_PLACEMENT_3D('',#17825,#14165,#14166);
#12030=AXIS2_PLACEMENT_3D('',#17827,#14167,#14168);
#12031=AXIS2_PLACEMENT_3D('',#17829,#14169,#14170);
#12032=AXIS2_PLACEMENT_3D('',#17830,#14171,#14172);
#12033=AXIS2_PLACEMENT_3D('',#17832,#14173,#14174);
#12034=AXIS2_PLACEMENT_3D('',#17834,#14176,#14177);
#12035=AXIS2_PLACEMENT_3D('',#17836,#14178,#14179);
#12036=AXIS2_PLACEMENT_3D('',#17837,#14180,#14181);
#12037=AXIS2_PLACEMENT_3D('',#17839,#14183,#14184);
#12038=AXIS2_PLACEMENT_3D('',#17841,#14185,#14186);
#12039=AXIS2_PLACEMENT_3D('',#17843,#14187,#14188);
#12040=AXIS2_PLACEMENT_3D('',#17844,#14189,#14190);
#12041=AXIS2_PLACEMENT_3D('',#17846,#14191,#14192);
#12042=AXIS2_PLACEMENT_3D('',#17848,#14194,#14195);
#12043=AXIS2_PLACEMENT_3D('',#17850,#14196,#14197);
#12044=AXIS2_PLACEMENT_3D('',#17851,#14198,#14199);
#12045=AXIS2_PLACEMENT_3D('',#17853,#14201,#14202);
#12046=AXIS2_PLACEMENT_3D('',#17854,#14203,#14204);
#12047=AXIS2_PLACEMENT_3D('',#17855,#14205,#14206);
#12048=AXIS2_PLACEMENT_3D('',#17856,#14207,#14208);
#12049=AXIS2_PLACEMENT_3D('',#17857,#14209,#14210);
#12050=AXIS2_PLACEMENT_3D('',#17858,#14211,#14212);
#12051=AXIS2_PLACEMENT_3D('',#17859,#14213,#14214);
#12052=AXIS2_PLACEMENT_3D('',#17868,#14219,#14220);
#12053=AXIS2_PLACEMENT_3D('',#17874,#14224,#14225);
#12054=AXIS2_PLACEMENT_3D('',#17880,#14229,#14230);
#12055=AXIS2_PLACEMENT_3D('',#17886,#14234,#14235);
#12056=AXIS2_PLACEMENT_3D('',#17892,#14239,#14240);
#12057=AXIS2_PLACEMENT_3D('',#17898,#14244,#14245);
#12058=AXIS2_PLACEMENT_3D('',#17904,#14249,#14250);
#12059=AXIS2_PLACEMENT_3D('',#17910,#14254,#14255);
#12060=AXIS2_PLACEMENT_3D('',#17916,#14259,#14260);
#12061=AXIS2_PLACEMENT_3D('',#17925,#14265,#14266);
#12062=AXIS2_PLACEMENT_3D('',#17931,#14270,#14271);
#12063=AXIS2_PLACEMENT_3D('',#17937,#14275,#14276);
#12064=AXIS2_PLACEMENT_3D('',#17943,#14280,#14281);
#12065=AXIS2_PLACEMENT_3D('',#17949,#14285,#14286);
#12066=AXIS2_PLACEMENT_3D('',#17955,#14290,#14291);
#12067=AXIS2_PLACEMENT_3D('',#17961,#14295,#14296);
#12068=AXIS2_PLACEMENT_3D('',#17967,#14300,#14301);
#12069=AXIS2_PLACEMENT_3D('',#17973,#14305,#14306);
#12070=AXIS2_PLACEMENT_3D('',#17982,#14311,#14312);
#12071=AXIS2_PLACEMENT_3D('',#17988,#14316,#14317);
#12072=AXIS2_PLACEMENT_3D('',#17994,#14321,#14322);
#12073=AXIS2_PLACEMENT_3D('',#18000,#14326,#14327);
#12074=AXIS2_PLACEMENT_3D('',#18006,#14331,#14332);
#12075=AXIS2_PLACEMENT_3D('',#18012,#14336,#14337);
#12076=AXIS2_PLACEMENT_3D('',#18018,#14341,#14342);
#12077=AXIS2_PLACEMENT_3D('',#18024,#14346,#14347);
#12078=AXIS2_PLACEMENT_3D('',#18030,#14351,#14352);
#12079=AXIS2_PLACEMENT_3D('',#18039,#14357,#14358);
#12080=AXIS2_PLACEMENT_3D('',#18045,#14362,#14363);
#12081=AXIS2_PLACEMENT_3D('',#18051,#14367,#14368);
#12082=AXIS2_PLACEMENT_3D('',#18057,#14372,#14373);
#12083=AXIS2_PLACEMENT_3D('',#18063,#14377,#14378);
#12084=AXIS2_PLACEMENT_3D('',#18069,#14382,#14383);
#12085=AXIS2_PLACEMENT_3D('',#18075,#14387,#14388);
#12086=AXIS2_PLACEMENT_3D('',#18081,#14392,#14393);
#12087=AXIS2_PLACEMENT_3D('',#18087,#14397,#14398);
#12088=AXIS2_PLACEMENT_3D('',#18089,#14399,#14400);
#12089=AXIS2_PLACEMENT_3D('',#18092,#14402,#14403);
#12090=AXIS2_PLACEMENT_3D('',#18093,#14404,#14405);
#12091=AXIS2_PLACEMENT_3D('',#18099,#14409,#14410);
#12092=AXIS2_PLACEMENT_3D('',#18105,#14414,#14415);
#12093=AXIS2_PLACEMENT_3D('',#18108,#14418,#14419);
#12094=AXIS2_PLACEMENT_3D('',#18114,#14423,#14424);
#12095=AXIS2_PLACEMENT_3D('',#18117,#14427,#14428);
#12096=AXIS2_PLACEMENT_3D('',#18123,#14432,#14433);
#12097=AXIS2_PLACEMENT_3D('',#18126,#14436,#14437);
#12098=AXIS2_PLACEMENT_3D('',#18129,#14440,#14441);
#12099=AXIS2_PLACEMENT_3D('',#18130,#14442,#14443);
#12100=AXIS2_PLACEMENT_3D('',#18131,#14444,#14445);
#12101=AXIS2_PLACEMENT_3D('',#18132,#14446,#14447);
#12102=AXIS2_PLACEMENT_3D('',#18141,#14452,#14453);
#12103=AXIS2_PLACEMENT_3D('',#18147,#14457,#14458);
#12104=AXIS2_PLACEMENT_3D('',#18154,#14462,#14463);
#12105=AXIS2_PLACEMENT_3D('',#18155,#14464,#14465);
#12106=AXIS2_PLACEMENT_3D('',#18169,#14473,#14474);
#12107=AXIS2_PLACEMENT_3D('',#18173,#14477,#14478);
#12108=AXIS2_PLACEMENT_3D('',#18177,#14481,#14482);
#12109=AXIS2_PLACEMENT_3D('',#18187,#14488,#14489);
#12110=AXIS2_PLACEMENT_3D('',#18189,#14491,#14492);
#12111=AXIS2_PLACEMENT_3D('',#18193,#14494,#14495);
#12112=AXIS2_PLACEMENT_3D('',#18195,#14497,#14498);
#12113=AXIS2_PLACEMENT_3D('',#18197,#14499,#14500);
#12114=AXIS2_PLACEMENT_3D('',#18200,#14502,#14503);
#12115=AXIS2_PLACEMENT_3D('',#18202,#14504,#14505);
#12116=AXIS2_PLACEMENT_3D('',#18203,#14506,#14507);
#12117=AXIS2_PLACEMENT_3D('',#18204,#14508,#14509);
#12118=AXIS2_PLACEMENT_3D('',#18206,#14511,#14512);
#12119=AXIS2_PLACEMENT_3D('',#18208,#14514,#14515);
#12120=AXIS2_PLACEMENT_3D('',#18210,#14517,#14518);
#12121=AXIS2_PLACEMENT_3D('',#18211,#14519,#14520);
#12122=AXIS2_PLACEMENT_3D('',#18212,#14521,#14522);
#12123=AXIS2_PLACEMENT_3D('',#18221,#14527,#14528);
#12124=AXIS2_PLACEMENT_3D('',#18227,#14532,#14533);
#12125=AXIS2_PLACEMENT_3D('',#18233,#14537,#14538);
#12126=AXIS2_PLACEMENT_3D('',#18239,#14542,#14543);
#12127=AXIS2_PLACEMENT_3D('',#18245,#14547,#14548);
#12128=AXIS2_PLACEMENT_3D('',#18248,#14551,#14552);
#12129=AXIS2_PLACEMENT_3D('',#18249,#14553,#14554);
#12130=AXIS2_PLACEMENT_3D('',#18250,#14555,#14556);
#12131=AXIS2_PLACEMENT_3D('',#18252,#14557,#14558);
#12132=AXIS2_PLACEMENT_3D('',#18253,#14559,#14560);
#12133=AXIS2_PLACEMENT_3D('',#18255,#14561,#14562);
#12134=AXIS2_PLACEMENT_3D('',#18256,#14563,#14564);
#12135=AXIS2_PLACEMENT_3D('',#18258,#14565,#14566);
#12136=AXIS2_PLACEMENT_3D('',#18260,#14568,#14569);
#12137=AXIS2_PLACEMENT_3D('',#18262,#14570,#14571);
#12138=AXIS2_PLACEMENT_3D('',#18264,#14573,#14574);
#12139=AXIS2_PLACEMENT_3D('',#18266,#14575,#14576);
#12140=AXIS2_PLACEMENT_3D('',#18268,#14578,#14579);
#12141=AXIS2_PLACEMENT_3D('',#18270,#14580,#14581);
#12142=AXIS2_PLACEMENT_3D('',#18271,#14582,#14583);
#12143=AXIS2_PLACEMENT_3D('',#18273,#14584,#14585);
#12144=AXIS2_PLACEMENT_3D('',#18275,#14587,#14588);
#12145=AXIS2_PLACEMENT_3D('',#18277,#14590,#14591);
#12146=AXIS2_PLACEMENT_3D('',#18278,#14592,#14593);
#12147=AXIS2_PLACEMENT_3D('',#18280,#14594,#14595);
#12148=AXIS2_PLACEMENT_3D('',#18283,#14597,#14598);
#12149=AXIS2_PLACEMENT_3D('',#18284,#14599,#14600);
#12150=AXIS2_PLACEMENT_3D('',#18286,#14601,#14602);
#12151=AXIS2_PLACEMENT_3D('',#18287,#14603,#14604);
#12152=AXIS2_PLACEMENT_3D('',#18289,#14605,#14606);
#12153=AXIS2_PLACEMENT_3D('',#18292,#14608,#14609);
#12154=AXIS2_PLACEMENT_3D('',#18293,#14610,#14611);
#12155=AXIS2_PLACEMENT_3D('',#18295,#14612,#14613);
#12156=AXIS2_PLACEMENT_3D('',#18296,#14614,#14615);
#12157=AXIS2_PLACEMENT_3D('',#18298,#14616,#14617);
#12158=AXIS2_PLACEMENT_3D('',#18301,#14619,#14620);
#12159=AXIS2_PLACEMENT_3D('',#18302,#14621,#14622);
#12160=AXIS2_PLACEMENT_3D('',#18304,#14623,#14624);
#12161=AXIS2_PLACEMENT_3D('',#18305,#14625,#14626);
#12162=AXIS2_PLACEMENT_3D('',#18307,#14627,#14628);
#12163=AXIS2_PLACEMENT_3D('',#18310,#14630,#14631);
#12164=AXIS2_PLACEMENT_3D('',#18311,#14632,#14633);
#12165=AXIS2_PLACEMENT_3D('',#18313,#14634,#14635);
#12166=AXIS2_PLACEMENT_3D('',#18314,#14636,#14637);
#12167=AXIS2_PLACEMENT_3D('',#18316,#14638,#14639);
#12168=AXIS2_PLACEMENT_3D('',#18318,#14641,#14642);
#12169=AXIS2_PLACEMENT_3D('',#18320,#14643,#14644);
#12170=AXIS2_PLACEMENT_3D('',#18322,#14646,#14647);
#12171=AXIS2_PLACEMENT_3D('',#18324,#14648,#14649);
#12172=AXIS2_PLACEMENT_3D('',#18326,#14651,#14652);
#12173=AXIS2_PLACEMENT_3D('',#18328,#14653,#14654);
#12174=AXIS2_PLACEMENT_3D('',#18330,#14656,#14657);
#12175=AXIS2_PLACEMENT_3D('',#18339,#14662,#14663);
#12176=AXIS2_PLACEMENT_3D('',#18345,#14667,#14668);
#12177=AXIS2_PLACEMENT_3D('',#18351,#14672,#14673);
#12178=AXIS2_PLACEMENT_3D('',#18357,#14677,#14678);
#12179=AXIS2_PLACEMENT_3D('',#18363,#14682,#14683);
#12180=AXIS2_PLACEMENT_3D('',#18369,#14687,#14688);
#12181=AXIS2_PLACEMENT_3D('',#18375,#14692,#14693);
#12182=AXIS2_PLACEMENT_3D('',#18381,#14697,#14698);
#12183=AXIS2_PLACEMENT_3D('',#18387,#14702,#14703);
#12184=AXIS2_PLACEMENT_3D('',#18393,#14707,#14708);
#12185=AXIS2_PLACEMENT_3D('',#18399,#14712,#14713);
#12186=AXIS2_PLACEMENT_3D('',#18402,#14716,#14717);
#12187=AXIS2_PLACEMENT_3D('',#18403,#14718,#14719);
#12188=AXIS2_PLACEMENT_3D('',#18404,#14720,#14721);
#12189=AXIS2_PLACEMENT_3D('',#18405,#14722,#14723);
#12190=AXIS2_PLACEMENT_3D('',#18406,#14724,#14725);
#12191=AXIS2_PLACEMENT_3D('',#18408,#14726,#14727);
#12192=AXIS2_PLACEMENT_3D('',#18411,#14729,#14730);
#12193=AXIS2_PLACEMENT_3D('',#18412,#14731,#14732);
#12194=AXIS2_PLACEMENT_3D('',#18413,#14733,#14734);
#12195=AXIS2_PLACEMENT_3D('',#18415,#14735,#14736);
#12196=AXIS2_PLACEMENT_3D('',#18417,#14737,#14738);
#12197=AXIS2_PLACEMENT_3D('',#18418,#14739,#14740);
#12198=AXIS2_PLACEMENT_3D('',#18420,#14741,#14742);
#12199=AXIS2_PLACEMENT_3D('',#18422,#14743,#14744);
#12200=AXIS2_PLACEMENT_3D('',#18423,#14745,#14746);
#12201=AXIS2_PLACEMENT_3D('',#18425,#14748,#14749);
#12202=AXIS2_PLACEMENT_3D('',#18428,#14751,#14752);
#12203=AXIS2_PLACEMENT_3D('',#18429,#14753,#14754);
#12204=AXIS2_PLACEMENT_3D('',#18431,#14755,#14756);
#12205=AXIS2_PLACEMENT_3D('',#18434,#14758,#14759);
#12206=AXIS2_PLACEMENT_3D('',#18435,#14760,#14761);
#12207=AXIS2_PLACEMENT_3D('',#18436,#14762,#14763);
#12208=AXIS2_PLACEMENT_3D('',#18438,#14764,#14765);
#12209=AXIS2_PLACEMENT_3D('',#18440,#14767,#14768);
#12210=AXIS2_PLACEMENT_3D('',#18441,#14769,#14770);
#12211=AXIS2_PLACEMENT_3D('',#18442,#14771,#14772);
#12212=AXIS2_PLACEMENT_3D('',#18443,#14773,#14774);
#12213=AXIS2_PLACEMENT_3D('',#18445,#14775,#14776);
#12214=AXIS2_PLACEMENT_3D('',#18448,#14778,#14779);
#12215=AXIS2_PLACEMENT_3D('',#18449,#14780,#14781);
#12216=AXIS2_PLACEMENT_3D('',#18451,#14782,#14783);
#12217=AXIS2_PLACEMENT_3D('',#18452,#14784,#14785);
#12218=AXIS2_PLACEMENT_3D('',#18455,#14787,#14788);
#12219=AXIS2_PLACEMENT_3D('',#18456,#14789,#14790);
#12220=AXIS2_PLACEMENT_3D('',#18458,#14791,#14792);
#12221=AXIS2_PLACEMENT_3D('',#18461,#14794,#14795);
#12222=AXIS2_PLACEMENT_3D('',#18462,#14796,#14797);
#12223=AXIS2_PLACEMENT_3D('',#18463,#14798,#14799);
#12224=AXIS2_PLACEMENT_3D('',#18464,#14800,#14801);
#12225=AXIS2_PLACEMENT_3D('',#18465,#14802,#14803);
#12226=AXIS2_PLACEMENT_3D('',#18467,#14804,#14805);
#12227=AXIS2_PLACEMENT_3D('',#18470,#14807,#14808);
#12228=AXIS2_PLACEMENT_3D('',#18471,#14809,#14810);
#12229=AXIS2_PLACEMENT_3D('',#18473,#14811,#14812);
#12230=AXIS2_PLACEMENT_3D('',#18476,#14814,#14815);
#12231=AXIS2_PLACEMENT_3D('',#18477,#14816,#14817);
#12232=AXIS2_PLACEMENT_3D('',#18478,#14818,#14819);
#12233=AXIS2_PLACEMENT_3D('',#18479,#14820,#14821);
#12234=AXIS2_PLACEMENT_3D('',#18480,#14822,#14823);
#12235=AXIS2_PLACEMENT_3D('',#18482,#14824,#14825);
#12236=AXIS2_PLACEMENT_3D('',#18485,#14827,#14828);
#12237=AXIS2_PLACEMENT_3D('',#18486,#14829,#14830);
#12238=AXIS2_PLACEMENT_3D('',#18487,#14831,#14832);
#12239=AXIS2_PLACEMENT_3D('',#18488,#14833,#14834);
#12240=AXIS2_PLACEMENT_3D('',#18489,#14835,#14836);
#12241=AXIS2_PLACEMENT_3D('',#18491,#14837,#14838);
#12242=AXIS2_PLACEMENT_3D('',#18494,#14840,#14841);
#12243=AXIS2_PLACEMENT_3D('',#18495,#14842,#14843);
#12244=AXIS2_PLACEMENT_3D('',#18496,#14844,#14845);
#12245=AXIS2_PLACEMENT_3D('',#18497,#14846,#14847);
#12246=AXIS2_PLACEMENT_3D('',#18498,#14848,#14849);
#12247=AXIS2_PLACEMENT_3D('',#18500,#14850,#14851);
#12248=AXIS2_PLACEMENT_3D('',#18503,#14853,#14854);
#12249=AXIS2_PLACEMENT_3D('',#18504,#14855,#14856);
#12250=AXIS2_PLACEMENT_3D('',#18506,#14857,#14858);
#12251=AXIS2_PLACEMENT_3D('',#18509,#14860,#14861);
#12252=AXIS2_PLACEMENT_3D('',#18510,#14862,#14863);
#12253=AXIS2_PLACEMENT_3D('',#18511,#14864,#14865);
#12254=AXIS2_PLACEMENT_3D('',#18512,#14866,#14867);
#12255=AXIS2_PLACEMENT_3D('',#18513,#14868,#14869);
#12256=AXIS2_PLACEMENT_3D('',#18514,#14870,#14871);
#12257=AXIS2_PLACEMENT_3D('',#18516,#14872,#14873);
#12258=AXIS2_PLACEMENT_3D('',#18519,#14875,#14876);
#12259=AXIS2_PLACEMENT_3D('',#18520,#14877,#14878);
#12260=AXIS2_PLACEMENT_3D('',#18521,#14879,#14880);
#12261=AXIS2_PLACEMENT_3D('',#18523,#14881,#14882);
#12262=AXIS2_PLACEMENT_3D('',#18525,#14883,#14884);
#12263=AXIS2_PLACEMENT_3D('',#18526,#14885,#14886);
#12264=AXIS2_PLACEMENT_3D('',#18528,#14887,#14888);
#12265=AXIS2_PLACEMENT_3D('',#18530,#14889,#14890);
#12266=AXIS2_PLACEMENT_3D('',#18531,#14891,#14892);
#12267=AXIS2_PLACEMENT_3D('',#18533,#14894,#14895);
#12268=AXIS2_PLACEMENT_3D('',#18536,#14897,#14898);
#12269=AXIS2_PLACEMENT_3D('',#18537,#14899,#14900);
#12270=AXIS2_PLACEMENT_3D('',#18539,#14901,#14902);
#12271=AXIS2_PLACEMENT_3D('',#18542,#14904,#14905);
#12272=AXIS2_PLACEMENT_3D('',#18543,#14906,#14907);
#12273=AXIS2_PLACEMENT_3D('',#18544,#14908,#14909);
#12274=AXIS2_PLACEMENT_3D('',#18546,#14910,#14911);
#12275=AXIS2_PLACEMENT_3D('',#18548,#14913,#14914);
#12276=AXIS2_PLACEMENT_3D('',#18549,#14915,#14916);
#12277=AXIS2_PLACEMENT_3D('',#18550,#14917,#14918);
#12278=AXIS2_PLACEMENT_3D('',#18551,#14919,#14920);
#12279=AXIS2_PLACEMENT_3D('',#18553,#14921,#14922);
#12280=AXIS2_PLACEMENT_3D('',#18556,#14924,#14925);
#12281=AXIS2_PLACEMENT_3D('',#18557,#14926,#14927);
#12282=AXIS2_PLACEMENT_3D('',#18559,#14928,#14929);
#12283=AXIS2_PLACEMENT_3D('',#18560,#14930,#14931);
#12284=AXIS2_PLACEMENT_3D('',#18563,#14933,#14934);
#12285=AXIS2_PLACEMENT_3D('',#18564,#14935,#14936);
#12286=AXIS2_PLACEMENT_3D('',#18566,#14937,#14938);
#12287=AXIS2_PLACEMENT_3D('',#18569,#14940,#14941);
#12288=AXIS2_PLACEMENT_3D('',#18570,#14942,#14943);
#12289=AXIS2_PLACEMENT_3D('',#18571,#14944,#14945);
#12290=AXIS2_PLACEMENT_3D('',#18572,#14946,#14947);
#12291=AXIS2_PLACEMENT_3D('',#18573,#14948,#14949);
#12292=AXIS2_PLACEMENT_3D('',#18575,#14950,#14951);
#12293=AXIS2_PLACEMENT_3D('',#18578,#14953,#14954);
#12294=AXIS2_PLACEMENT_3D('',#18579,#14955,#14956);
#12295=AXIS2_PLACEMENT_3D('',#18581,#14957,#14958);
#12296=AXIS2_PLACEMENT_3D('',#18584,#14960,#14961);
#12297=AXIS2_PLACEMENT_3D('',#18585,#14962,#14963);
#12298=AXIS2_PLACEMENT_3D('',#18586,#14964,#14965);
#12299=AXIS2_PLACEMENT_3D('',#18587,#14966,#14967);
#12300=AXIS2_PLACEMENT_3D('',#18588,#14968,#14969);
#12301=AXIS2_PLACEMENT_3D('',#18590,#14970,#14971);
#12302=AXIS2_PLACEMENT_3D('',#18593,#14973,#14974);
#12303=AXIS2_PLACEMENT_3D('',#18594,#14975,#14976);
#12304=AXIS2_PLACEMENT_3D('',#18595,#14977,#14978);
#12305=AXIS2_PLACEMENT_3D('',#18596,#14979,#14980);
#12306=AXIS2_PLACEMENT_3D('',#18597,#14981,#14982);
#12307=AXIS2_PLACEMENT_3D('',#18599,#14983,#14984);
#12308=AXIS2_PLACEMENT_3D('',#18602,#14986,#14987);
#12309=AXIS2_PLACEMENT_3D('',#18603,#14988,#14989);
#12310=AXIS2_PLACEMENT_3D('',#18604,#14990,#14991);
#12311=AXIS2_PLACEMENT_3D('',#18605,#14992,#14993);
#12312=AXIS2_PLACEMENT_3D('',#18606,#14994,#14995);
#12313=AXIS2_PLACEMENT_3D('',#18608,#14996,#14997);
#12314=AXIS2_PLACEMENT_3D('',#18611,#14999,#15000);
#12315=AXIS2_PLACEMENT_3D('',#18612,#15001,#15002);
#12316=AXIS2_PLACEMENT_3D('',#18614,#15003,#15004);
#12317=AXIS2_PLACEMENT_3D('',#18617,#15006,#15007);
#12318=AXIS2_PLACEMENT_3D('',#18618,#15008,#15009);
#12319=AXIS2_PLACEMENT_3D('',#18619,#15010,#15011);
#12320=AXIS2_PLACEMENT_3D('',#18620,#15012,#15013);
#12321=AXIS2_PLACEMENT_3D('',#18621,#15014,#15015);
#12322=AXIS2_PLACEMENT_3D('',#18708,#15017,#15018);
#12323=AXIS2_PLACEMENT_3D('',#18789,#15020,#15021);
#12324=AXIS2_PLACEMENT_3D('',#18791,#15022,#15023);
#12325=AXIS2_PLACEMENT_3D('',#18795,#15026,#15027);
#12326=AXIS2_PLACEMENT_3D('',#18878,#15028,#15029);
#12327=AXIS2_PLACEMENT_3D('',#18918,#15031,#15032);
#12328=AXIS2_PLACEMENT_3D('',#18958,#15034,#15035);
#12329=AXIS2_PLACEMENT_3D('',#18960,#15036,#15037);
#12330=AXIS2_PLACEMENT_3D('',#18964,#15040,#15041);
#12331=AXIS2_PLACEMENT_3D('',#18965,#15042,#15043);
#12332=AXIS2_PLACEMENT_3D('',#18966,#15044,#15045);
#12333=AXIS2_PLACEMENT_3D('',#18968,#15046,#15047);
#12334=AXIS2_PLACEMENT_3D('',#18971,#15048,#15049);
#12335=AXIS2_PLACEMENT_3D('',#18973,#15050,#15051);
#12336=AXIS2_PLACEMENT_3D('',#18975,#15052,#15053);
#12337=AXIS2_PLACEMENT_3D('',#18977,#15054,#15055);
#12338=AXIS2_PLACEMENT_3D('',#18979,#15056,#15057);
#12339=AXIS2_PLACEMENT_3D('',#18981,#15058,#15059);
#12340=AXIS2_PLACEMENT_3D('',#18983,#15060,#15061);
#12341=AXIS2_PLACEMENT_3D('',#18985,#15062,#15063);
#12342=AXIS2_PLACEMENT_3D('',#18987,#15064,#15065);
#12343=AXIS2_PLACEMENT_3D('',#18989,#15066,#15067);
#12344=AXIS2_PLACEMENT_3D('',#18991,#15068,#15069);
#12345=AXIS2_PLACEMENT_3D('',#18993,#15070,#15071);
#12346=AXIS2_PLACEMENT_3D('',#18995,#15072,#15073);
#12347=AXIS2_PLACEMENT_3D('',#18997,#15074,#15075);
#12348=AXIS2_PLACEMENT_3D('',#18999,#15076,#15077);
#12349=AXIS2_PLACEMENT_3D('',#19001,#15078,#15079);
#12350=AXIS2_PLACEMENT_3D('',#19003,#15080,#15081);
#12351=AXIS2_PLACEMENT_3D('',#19005,#15082,#15083);
#12352=AXIS2_PLACEMENT_3D('',#19007,#15084,#15085);
#12353=AXIS2_PLACEMENT_3D('',#19009,#15086,#15087);
#12354=AXIS2_PLACEMENT_3D('',#19011,#15088,#15089);
#12355=AXIS2_PLACEMENT_3D('',#19013,#15090,#15091);
#12356=AXIS2_PLACEMENT_3D('',#19015,#15092,#15093);
#12357=AXIS2_PLACEMENT_3D('',#19017,#15094,#15095);
#12358=AXIS2_PLACEMENT_3D('',#19019,#15096,#15097);
#12359=AXIS2_PLACEMENT_3D('',#19021,#15098,#15099);
#12360=AXIS2_PLACEMENT_3D('',#19023,#15100,#15101);
#12361=AXIS2_PLACEMENT_3D('',#19025,#15102,#15103);
#12362=AXIS2_PLACEMENT_3D('',#19027,#15104,#15105);
#12363=AXIS2_PLACEMENT_3D('',#19029,#15106,#15107);
#12364=AXIS2_PLACEMENT_3D('',#19031,#15108,#15109);
#12365=AXIS2_PLACEMENT_3D('',#19033,#15110,#15111);
#12366=AXIS2_PLACEMENT_3D('',#19035,#15112,#15113);
#12367=AXIS2_PLACEMENT_3D('',#19037,#15114,#15115);
#12368=AXIS2_PLACEMENT_3D('',#19039,#15116,#15117);
#12369=AXIS2_PLACEMENT_3D('',#19041,#15118,#15119);
#12370=AXIS2_PLACEMENT_3D('',#19043,#15120,#15121);
#12371=AXIS2_PLACEMENT_3D('',#19045,#15122,#15123);
#12372=AXIS2_PLACEMENT_3D('',#19047,#15124,#15125);
#12373=AXIS2_PLACEMENT_3D('',#19048,#15126,#15127);
#12374=AXIS2_PLACEMENT_3D('',#19049,#15128,#15129);
#12375=AXIS2_PLACEMENT_3D('',#19051,#15130,#15131);
#12376=AXIS2_PLACEMENT_3D('',#19053,#15133,#15134);
#12377=AXIS2_PLACEMENT_3D('',#19054,#15135,#15136);
#12378=AXIS2_PLACEMENT_3D('',#19056,#15137,#15138);
#12379=AXIS2_PLACEMENT_3D('',#19059,#15139,#15140);
#12380=AXIS2_PLACEMENT_3D('',#19061,#15141,#15142);
#12381=AXIS2_PLACEMENT_3D('',#19063,#15143,#15144);
#12382=AXIS2_PLACEMENT_3D('',#19065,#15145,#15146);
#12383=AXIS2_PLACEMENT_3D('',#19067,#15147,#15148);
#12384=AXIS2_PLACEMENT_3D('',#19069,#15149,#15150);
#12385=AXIS2_PLACEMENT_3D('',#19071,#15151,#15152);
#12386=AXIS2_PLACEMENT_3D('',#19073,#15153,#15154);
#12387=AXIS2_PLACEMENT_3D('',#19075,#15155,#15156);
#12388=AXIS2_PLACEMENT_3D('',#19077,#15157,#15158);
#12389=AXIS2_PLACEMENT_3D('',#19079,#15159,#15160);
#12390=AXIS2_PLACEMENT_3D('',#19081,#15161,#15162);
#12391=AXIS2_PLACEMENT_3D('',#19083,#15163,#15164);
#12392=AXIS2_PLACEMENT_3D('',#19085,#15165,#15166);
#12393=AXIS2_PLACEMENT_3D('',#19087,#15167,#15168);
#12394=AXIS2_PLACEMENT_3D('',#19089,#15169,#15170);
#12395=AXIS2_PLACEMENT_3D('',#19091,#15171,#15172);
#12396=AXIS2_PLACEMENT_3D('',#19093,#15173,#15174);
#12397=AXIS2_PLACEMENT_3D('',#19095,#15175,#15176);
#12398=AXIS2_PLACEMENT_3D('',#19097,#15177,#15178);
#12399=AXIS2_PLACEMENT_3D('',#19099,#15179,#15180);
#12400=AXIS2_PLACEMENT_3D('',#19101,#15181,#15182);
#12401=AXIS2_PLACEMENT_3D('',#19103,#15183,#15184);
#12402=AXIS2_PLACEMENT_3D('',#19105,#15185,#15186);
#12403=AXIS2_PLACEMENT_3D('',#19107,#15187,#15188);
#12404=AXIS2_PLACEMENT_3D('',#19109,#15189,#15190);
#12405=AXIS2_PLACEMENT_3D('',#19111,#15191,#15192);
#12406=AXIS2_PLACEMENT_3D('',#19113,#15193,#15194);
#12407=AXIS2_PLACEMENT_3D('',#19115,#15195,#15196);
#12408=AXIS2_PLACEMENT_3D('',#19117,#15197,#15198);
#12409=AXIS2_PLACEMENT_3D('',#19119,#15199,#15200);
#12410=AXIS2_PLACEMENT_3D('',#19121,#15201,#15202);
#12411=AXIS2_PLACEMENT_3D('',#19123,#15203,#15204);
#12412=AXIS2_PLACEMENT_3D('',#19125,#15205,#15206);
#12413=AXIS2_PLACEMENT_3D('',#19127,#15207,#15208);
#12414=AXIS2_PLACEMENT_3D('',#19129,#15209,#15210);
#12415=AXIS2_PLACEMENT_3D('',#19131,#15211,#15212);
#12416=AXIS2_PLACEMENT_3D('',#19133,#15213,#15214);
#12417=AXIS2_PLACEMENT_3D('',#19135,#15215,#15216);
#12418=AXIS2_PLACEMENT_3D('',#19136,#15217,#15218);
#12419=AXIS2_PLACEMENT_3D('',#19137,#15219,#15220);
#12420=AXIS2_PLACEMENT_3D('',#19139,#15221,#15222);
#12421=AXIS2_PLACEMENT_3D('',#19141,#15224,#15225);
#12422=AXIS2_PLACEMENT_3D('',#19142,#15226,#15227);
#12423=AXIS2_PLACEMENT_3D('',#19145,#15230,#15231);
#12424=AXIS2_PLACEMENT_3D('',#19147,#15233,#15234);
#12425=AXIS2_PLACEMENT_3D('',#19149,#15236,#15237);
#12426=AXIS2_PLACEMENT_3D('',#19151,#15239,#15240);
#12427=AXIS2_PLACEMENT_3D('',#19153,#15242,#15243);
#12428=AXIS2_PLACEMENT_3D('',#19155,#15245,#15246);
#12429=AXIS2_PLACEMENT_3D('',#19157,#15248,#15249);
#12430=AXIS2_PLACEMENT_3D('',#19159,#15251,#15252);
#12431=AXIS2_PLACEMENT_3D('',#19161,#15254,#15255);
#12432=AXIS2_PLACEMENT_3D('',#19163,#15257,#15258);
#12433=AXIS2_PLACEMENT_3D('',#19165,#15260,#15261);
#12434=AXIS2_PLACEMENT_3D('',#19167,#15263,#15264);
#12435=AXIS2_PLACEMENT_3D('',#19169,#15266,#15267);
#12436=AXIS2_PLACEMENT_3D('',#19171,#15269,#15270);
#12437=AXIS2_PLACEMENT_3D('',#19173,#15272,#15273);
#12438=AXIS2_PLACEMENT_3D('',#19175,#15275,#15276);
#12439=AXIS2_PLACEMENT_3D('',#19177,#15278,#15279);
#12440=AXIS2_PLACEMENT_3D('',#19179,#15281,#15282);
#12441=AXIS2_PLACEMENT_3D('',#19181,#15284,#15285);
#12442=AXIS2_PLACEMENT_3D('',#19183,#15287,#15288);
#12443=AXIS2_PLACEMENT_3D('',#19185,#15290,#15291);
#12444=AXIS2_PLACEMENT_3D('',#19187,#15293,#15294);
#12445=AXIS2_PLACEMENT_3D('',#19189,#15296,#15297);
#12446=AXIS2_PLACEMENT_3D('',#19191,#15299,#15300);
#12447=AXIS2_PLACEMENT_3D('',#19193,#15302,#15303);
#12448=AXIS2_PLACEMENT_3D('',#19195,#15305,#15306);
#12449=AXIS2_PLACEMENT_3D('',#19197,#15308,#15309);
#12450=AXIS2_PLACEMENT_3D('',#19199,#15311,#15312);
#12451=AXIS2_PLACEMENT_3D('',#19201,#15314,#15315);
#12452=AXIS2_PLACEMENT_3D('',#19203,#15317,#15318);
#12453=AXIS2_PLACEMENT_3D('',#19205,#15320,#15321);
#12454=AXIS2_PLACEMENT_3D('',#19207,#15323,#15324);
#12455=AXIS2_PLACEMENT_3D('',#19209,#15326,#15327);
#12456=AXIS2_PLACEMENT_3D('',#19211,#15329,#15330);
#12457=AXIS2_PLACEMENT_3D('',#19213,#15332,#15333);
#12458=AXIS2_PLACEMENT_3D('',#19215,#15335,#15336);
#12459=AXIS2_PLACEMENT_3D('',#19217,#15338,#15339);
#12460=AXIS2_PLACEMENT_3D('',#19219,#15341,#15342);
#12461=AXIS2_PLACEMENT_3D('',#19221,#15344,#15345);
#12462=AXIS2_PLACEMENT_3D('',#19222,#15346,#15347);
#12463=AXIS2_PLACEMENT_3D('',#19223,#15348,#15349);
#12464=AXIS2_PLACEMENT_3D('',#19224,#15350,#15351);
#12465=AXIS2_PLACEMENT_3D('',#19226,#15352,#15353);
#12466=AXIS2_PLACEMENT_3D('',#19229,#15355,#15356);
#12467=AXIS2_PLACEMENT_3D('',#19230,#15357,#15358);
#12468=AXIS2_PLACEMENT_3D('',#19232,#15359,#15360);
#12469=AXIS2_PLACEMENT_3D('',#19233,#15361,#15362);
#12470=AXIS2_PLACEMENT_3D('',#19235,#15363,#15364);
#12471=AXIS2_PLACEMENT_3D('',#19238,#15366,#15367);
#12472=AXIS2_PLACEMENT_3D('',#19239,#15368,#15369);
#12473=AXIS2_PLACEMENT_3D('',#19241,#15370,#15371);
#12474=AXIS2_PLACEMENT_3D('',#19242,#15372,#15373);
#12475=AXIS2_PLACEMENT_3D('',#19245,#15375,#15376);
#12476=AXIS2_PLACEMENT_3D('',#19246,#15377,#15378);
#12477=AXIS2_PLACEMENT_3D('',#19249,#15380,#15381);
#12478=AXIS2_PLACEMENT_3D('',#19250,#15382,#15383);
#12479=AXIS2_PLACEMENT_3D('',#19252,#15384,#15385);
#12480=AXIS2_PLACEMENT_3D('',#19255,#15387,#15388);
#12481=AXIS2_PLACEMENT_3D('',#19256,#15389,#15390);
#12482=AXIS2_PLACEMENT_3D('',#19258,#15391,#15392);
#12483=AXIS2_PLACEMENT_3D('',#19261,#15394,#15395);
#12484=AXIS2_PLACEMENT_3D('',#19262,#15396,#15397);
#12485=AXIS2_PLACEMENT_3D('',#19264,#15398,#15399);
#12486=AXIS2_PLACEMENT_3D('',#19267,#15401,#15402);
#12487=AXIS2_PLACEMENT_3D('',#19268,#15403,#15404);
#12488=AXIS2_PLACEMENT_3D('',#19270,#15405,#15406);
#12489=AXIS2_PLACEMENT_3D('',#19273,#15408,#15409);
#12490=AXIS2_PLACEMENT_3D('',#19274,#15410,#15411);
#12491=AXIS2_PLACEMENT_3D('',#19283,#15416,#15417);
#12492=AXIS2_PLACEMENT_3D('',#19289,#15421,#15422);
#12493=AXIS2_PLACEMENT_3D('',#19295,#15426,#15427);
#12494=AXIS2_PLACEMENT_3D('',#19298,#15430,#15431);
#12495=AXIS2_PLACEMENT_3D('',#19299,#15432,#15433);
#12496=AXIS2_PLACEMENT_3D('',#19300,#15434,#15435);
#12497=AXIS2_PLACEMENT_3D('',#19301,#15436,#15437);
#12498=AXIS2_PLACEMENT_3D('',#19303,#15438,#15439);
#12499=AXIS2_PLACEMENT_3D('',#19306,#15441,#15442);
#12500=AXIS2_PLACEMENT_3D('',#19307,#15443,#15444);
#12501=AXIS2_PLACEMENT_3D('',#19308,#15445,#15446);
#12502=AXIS2_PLACEMENT_3D('',#19310,#15447,#15448);
#12503=AXIS2_PLACEMENT_3D('',#19313,#15450,#15451);
#12504=AXIS2_PLACEMENT_3D('',#19314,#15452,#15453);
#12505=AXIS2_PLACEMENT_3D('',#19315,#15454,#15455);
#12506=AXIS2_PLACEMENT_3D('',#19320,#15457,#15458);
#12507=AXIS2_PLACEMENT_3D('',#19324,#15461,#15462);
#12508=AXIS2_PLACEMENT_3D('',#19328,#15464,#15465);
#12509=AXIS2_PLACEMENT_3D('',#19330,#15467,#15468);
#12510=AXIS2_PLACEMENT_3D('',#19335,#15470,#15471);
#12511=AXIS2_PLACEMENT_3D('',#19338,#15473,#15474);
#12512=AXIS2_PLACEMENT_3D('',#19339,#15475,#15476);
#12513=AXIS2_PLACEMENT_3D('',#19345,#15480,#15481);
#12514=AXIS2_PLACEMENT_3D('',#19355,#15487,#15488);
#12515=AXIS2_PLACEMENT_3D('',#19360,#15492,#15493);
#12516=AXIS2_PLACEMENT_3D('',#19362,#15494,#15495);
#12517=AXIS2_PLACEMENT_3D('',#19365,#15497,#15498);
#12518=AXIS2_PLACEMENT_3D('',#19366,#15499,#15500);
#12519=AXIS2_PLACEMENT_3D('',#19367,#15501,#15502);
#12520=AXIS2_PLACEMENT_3D('',#19369,#15503,#15504);
#12521=AXIS2_PLACEMENT_3D('',#19372,#15506,#15507);
#12522=AXIS2_PLACEMENT_3D('',#19373,#15508,#15509);
#12523=AXIS2_PLACEMENT_3D('',#19374,#15510,#15511);
#12524=AXIS2_PLACEMENT_3D('',#19380,#15515,#15516);
#12525=AXIS2_PLACEMENT_3D('',#19384,#15519,#15520);
#12526=AXIS2_PLACEMENT_3D('',#19386,#15522,#15523);
#12527=AXIS2_PLACEMENT_3D('',#19389,#15526,#15527);
#12528=AXIS2_PLACEMENT_3D('',#19390,#15528,#15529);
#12529=AXIS2_PLACEMENT_3D('',#19391,#15530,#15531);
#12530=AXIS2_PLACEMENT_3D('',#19392,#15532,#15533);
#12531=AXIS2_PLACEMENT_3D('',#19401,#15538,#15539);
#12532=AXIS2_PLACEMENT_3D('',#19407,#15543,#15544);
#12533=AXIS2_PLACEMENT_3D('',#19413,#15548,#15549);
#12534=AXIS2_PLACEMENT_3D('',#19416,#15552,#15553);
#12535=AXIS2_PLACEMENT_3D('',#19417,#15554,#15555);
#12536=AXIS2_PLACEMENT_3D('',#19418,#15556,#15557);
#12537=AXIS2_PLACEMENT_3D('',#19419,#15558,#15559);
#12538=AXIS2_PLACEMENT_3D('',#19420,#15560,#15561);
#12539=AXIS2_PLACEMENT_3D('',#19424,#15563,#15564);
#12540=AXIS2_PLACEMENT_3D('',#19425,#15565,#15566);
#12541=AXIS2_PLACEMENT_3D('',#19429,#15568,#15569);
#12542=AXIS2_PLACEMENT_3D('',#19432,#15571,#15572);
#12543=AXIS2_PLACEMENT_3D('',#19434,#15573,#15574);
#12544=AXIS2_PLACEMENT_3D('',#19436,#15576,#15577);
#12545=AXIS2_PLACEMENT_3D('',#19440,#15579,#15580);
#12546=AXIS2_PLACEMENT_3D('',#19441,#15581,#15582);
#12547=AXIS2_PLACEMENT_3D('',#19445,#15584,#15585);
#12548=AXIS2_PLACEMENT_3D('',#19448,#15587,#15588);
#12549=AXIS2_PLACEMENT_3D('',#19450,#15589,#15590);
#12550=AXIS2_PLACEMENT_3D('',#19452,#15592,#15593);
#12551=AXIS2_PLACEMENT_3D('',#19456,#15595,#15596);
#12552=AXIS2_PLACEMENT_3D('',#19457,#15597,#15598);
#12553=AXIS2_PLACEMENT_3D('',#19461,#15600,#15601);
#12554=AXIS2_PLACEMENT_3D('',#19464,#15603,#15604);
#12555=AXIS2_PLACEMENT_3D('',#19466,#15605,#15606);
#12556=AXIS2_PLACEMENT_3D('',#19468,#15608,#15609);
#12557=AXIS2_PLACEMENT_3D('',#19472,#15611,#15612);
#12558=AXIS2_PLACEMENT_3D('',#19473,#15613,#15614);
#12559=AXIS2_PLACEMENT_3D('',#19477,#15616,#15617);
#12560=AXIS2_PLACEMENT_3D('',#19480,#15619,#15620);
#12561=AXIS2_PLACEMENT_3D('',#19482,#15621,#15622);
#12562=AXIS2_PLACEMENT_3D('',#19484,#15624,#15625);
#12563=AXIS2_PLACEMENT_3D('',#19495,#15632,#15633);
#12564=AXIS2_PLACEMENT_3D('',#19506,#15640,#15641);
#12565=AXIS2_PLACEMENT_3D('',#19525,#15652,#15653);
#12566=AXIS2_PLACEMENT_3D('',#19529,#15656,#15657);
#12567=AXIS2_PLACEMENT_3D('',#19533,#15660,#15661);
#12568=AXIS2_PLACEMENT_3D('',#19537,#15664,#15665);
#12569=AXIS2_PLACEMENT_3D('',#19541,#15668,#15669);
#12570=AXIS2_PLACEMENT_3D('',#19543,#15671,#15672);
#12571=AXIS2_PLACEMENT_3D('',#19547,#15675,#15676);
#12572=AXIS2_PLACEMENT_3D('',#19551,#15679,#15680);
#12573=AXIS2_PLACEMENT_3D('',#19555,#15683,#15684);
#12574=AXIS2_PLACEMENT_3D('',#19559,#15687,#15688);
#12575=AXIS2_PLACEMENT_3D('',#19561,#15690,#15691);
#12576=AXIS2_PLACEMENT_3D('',#19562,#15692,#15693);
#12577=AXIS2_PLACEMENT_3D('',#19563,#15694,#15695);
#12578=AXIS2_PLACEMENT_3D('',#19572,#15700,#15701);
#12579=AXIS2_PLACEMENT_3D('',#19578,#15705,#15706);
#12580=AXIS2_PLACEMENT_3D('',#19584,#15710,#15711);
#12581=AXIS2_PLACEMENT_3D('',#19590,#15715,#15716);
#12582=AXIS2_PLACEMENT_3D('',#19596,#15720,#15721);
#12583=AXIS2_PLACEMENT_3D('',#19602,#15725,#15726);
#12584=AXIS2_PLACEMENT_3D('',#19608,#15730,#15731);
#12585=AXIS2_PLACEMENT_3D('',#19611,#15734,#15735);
#12586=AXIS2_PLACEMENT_3D('',#19612,#15736,#15737);
#12587=AXIS2_PLACEMENT_3D('',#19613,#15738,#15739);
#12588=AXIS2_PLACEMENT_3D('',#19614,#15740,#15741);
#12589=AXIS2_PLACEMENT_3D('',#19623,#15746,#15747);
#12590=AXIS2_PLACEMENT_3D('',#19629,#15751,#15752);
#12591=AXIS2_PLACEMENT_3D('',#19635,#15756,#15757);
#12592=AXIS2_PLACEMENT_3D('',#19641,#15761,#15762);
#12593=AXIS2_PLACEMENT_3D('',#19647,#15766,#15767);
#12594=AXIS2_PLACEMENT_3D('',#19653,#15771,#15772);
#12595=AXIS2_PLACEMENT_3D('',#19659,#15776,#15777);
#12596=AXIS2_PLACEMENT_3D('',#19662,#15780,#15781);
#12597=AXIS2_PLACEMENT_3D('',#19663,#15782,#15783);
#12598=AXIS2_PLACEMENT_3D('',#19664,#15784,#15785);
#12599=AXIS2_PLACEMENT_3D('',#19665,#15786,#15787);
#12600=AXIS2_PLACEMENT_3D('',#19666,#15788,#15789);
#12601=AXIS2_PLACEMENT_3D('',#19667,#15790,#15791);
#12602=AXIS2_PLACEMENT_3D('',#19668,#15792,#15793);
#12603=AXIS2_PLACEMENT_3D('',#19670,#15794,#15795);
#12604=AXIS2_PLACEMENT_3D('',#19673,#15797,#15798);
#12605=AXIS2_PLACEMENT_3D('',#19674,#15799,#15800);
#12606=AXIS2_PLACEMENT_3D('',#19677,#15802,#15803);
#12607=AXIS2_PLACEMENT_3D('',#19678,#15804,#15805);
#12608=AXIS2_PLACEMENT_3D('',#19680,#15806,#15807);
#12609=AXIS2_PLACEMENT_3D('',#19681,#15808,#15809);
#12610=AXIS2_PLACEMENT_3D('',#19684,#15811,#15812);
#12611=AXIS2_PLACEMENT_3D('',#19685,#15813,#15814);
#12612=AXIS2_PLACEMENT_3D('',#19686,#15815,#15816);
#12613=AXIS2_PLACEMENT_3D('',#19687,#15817,#15818);
#12614=AXIS2_PLACEMENT_3D('',#19689,#15819,#15820);
#12615=AXIS2_PLACEMENT_3D('',#19690,#15821,#15822);
#12616=AXIS2_PLACEMENT_3D('',#19692,#15823,#15824);
#12617=AXIS2_PLACEMENT_3D('',#19694,#15826,#15827);
#12618=AXIS2_PLACEMENT_3D('',#19696,#15828,#15829);
#12619=AXIS2_PLACEMENT_3D('',#19698,#15831,#15832);
#12620=AXIS2_PLACEMENT_3D('',#19700,#15833,#15834);
#12621=AXIS2_PLACEMENT_3D('',#19702,#15836,#15837);
#12622=AXIS2_PLACEMENT_3D('',#19704,#15838,#15839);
#12623=AXIS2_PLACEMENT_3D('',#19705,#15840,#15841);
#12624=AXIS2_PLACEMENT_3D('',#19707,#15842,#15843);
#12625=AXIS2_PLACEMENT_3D('',#19709,#15845,#15846);
#12626=AXIS2_PLACEMENT_3D('',#19711,#15847,#15848);
#12627=AXIS2_PLACEMENT_3D('',#19713,#15850,#15851);
#12628=AXIS2_PLACEMENT_3D('',#19715,#15852,#15853);
#12629=AXIS2_PLACEMENT_3D('',#19717,#15855,#15856);
#12630=AXIS2_PLACEMENT_3D('',#19718,#15857,#15858);
#12631=AXIS2_PLACEMENT_3D('',#19727,#15863,#15864);
#12632=AXIS2_PLACEMENT_3D('',#19733,#15868,#15869);
#12633=AXIS2_PLACEMENT_3D('',#19739,#15873,#15874);
#12634=AXIS2_PLACEMENT_3D('',#19745,#15878,#15879);
#12635=AXIS2_PLACEMENT_3D('',#19751,#15883,#15884);
#12636=AXIS2_PLACEMENT_3D('',#19754,#15887,#15888);
#12637=AXIS2_PLACEMENT_3D('',#19755,#15889,#15890);
#12638=AXIS2_PLACEMENT_3D('',#19756,#15891,#15892);
#12639=AXIS2_PLACEMENT_3D('',#19757,#15893,#15894);
#12640=AXIS2_PLACEMENT_3D('',#19766,#15899,#15900);
#12641=AXIS2_PLACEMENT_3D('',#19772,#15904,#15905);
#12642=AXIS2_PLACEMENT_3D('',#19778,#15909,#15910);
#12643=AXIS2_PLACEMENT_3D('',#19784,#15914,#15915);
#12644=AXIS2_PLACEMENT_3D('',#19790,#15919,#15920);
#12645=AXIS2_PLACEMENT_3D('',#19793,#15923,#15924);
#12646=AXIS2_PLACEMENT_3D('',#19794,#15925,#15926);
#12647=AXIS2_PLACEMENT_3D('',#19795,#15927,#15928);
#12648=AXIS2_PLACEMENT_3D('',#19797,#15929,#15930);
#12649=AXIS2_PLACEMENT_3D('',#19798,#15931,#15932);
#12650=AXIS2_PLACEMENT_3D('',#19800,#15933,#15934);
#12651=AXIS2_PLACEMENT_3D('',#19801,#15935,#15936);
#12652=AXIS2_PLACEMENT_3D('',#19803,#15937,#15938);
#12653=AXIS2_PLACEMENT_3D('',#19805,#15940,#15941);
#12654=AXIS2_PLACEMENT_3D('',#19807,#15942,#15943);
#12655=AXIS2_PLACEMENT_3D('',#19809,#15945,#15946);
#12656=AXIS2_PLACEMENT_3D('',#19811,#15947,#15948);
#12657=AXIS2_PLACEMENT_3D('',#19813,#15950,#15951);
#12658=AXIS2_PLACEMENT_3D('',#19815,#15952,#15953);
#12659=AXIS2_PLACEMENT_3D('',#19816,#15954,#15955);
#12660=AXIS2_PLACEMENT_3D('',#19818,#15956,#15957);
#12661=AXIS2_PLACEMENT_3D('',#19820,#15959,#15960);
#12662=AXIS2_PLACEMENT_3D('',#19822,#15962,#15963);
#12663=AXIS2_PLACEMENT_3D('',#19823,#15964,#15965);
#12664=AXIS2_PLACEMENT_3D('',#19825,#15966,#15967);
#12665=AXIS2_PLACEMENT_3D('',#19826,#15968,#15969);
#12666=AXIS2_PLACEMENT_3D('',#19828,#15970,#15971);
#12667=AXIS2_PLACEMENT_3D('',#19830,#15973,#15974);
#12668=AXIS2_PLACEMENT_3D('',#19832,#15975,#15976);
#12669=AXIS2_PLACEMENT_3D('',#19834,#15978,#15979);
#12670=AXIS2_PLACEMENT_3D('',#19836,#15980,#15981);
#12671=AXIS2_PLACEMENT_3D('',#19838,#15983,#15984);
#12672=AXIS2_PLACEMENT_3D('',#19840,#15985,#15986);
#12673=AXIS2_PLACEMENT_3D('',#19841,#15987,#15988);
#12674=AXIS2_PLACEMENT_3D('',#19843,#15989,#15990);
#12675=AXIS2_PLACEMENT_3D('',#19845,#15992,#15993);
#12676=AXIS2_PLACEMENT_3D('',#19847,#15994,#15995);
#12677=AXIS2_PLACEMENT_3D('',#19849,#15997,#15998);
#12678=AXIS2_PLACEMENT_3D('',#19851,#15999,#16000);
#12679=AXIS2_PLACEMENT_3D('',#19853,#16002,#16003);
#12680=AXIS2_PLACEMENT_3D('',#19854,#16004,#16005);
#12681=AXIS2_PLACEMENT_3D('',#19863,#16010,#16011);
#12682=AXIS2_PLACEMENT_3D('',#19869,#16015,#16016);
#12683=AXIS2_PLACEMENT_3D('',#19875,#16020,#16021);
#12684=AXIS2_PLACEMENT_3D('',#19881,#16025,#16026);
#12685=AXIS2_PLACEMENT_3D('',#19887,#16030,#16031);
#12686=AXIS2_PLACEMENT_3D('',#19890,#16034,#16035);
#12687=AXIS2_PLACEMENT_3D('',#19891,#16036,#16037);
#12688=AXIS2_PLACEMENT_3D('',#19892,#16038,#16039);
#12689=AXIS2_PLACEMENT_3D('',#19893,#16040,#16041);
#12690=AXIS2_PLACEMENT_3D('',#19894,#16042,#16043);
#12691=AXIS2_PLACEMENT_3D('',#19895,#16044,#16045);
#12692=AXIS2_PLACEMENT_3D('',#19896,#16046,#16047);
#12693=AXIS2_PLACEMENT_3D('',#19897,#16048,#16049);
#12694=AXIS2_PLACEMENT_3D('',#19898,#16050,#16051);
#12695=AXIS2_PLACEMENT_3D('',#19899,#16052,#16053);
#12696=AXIS2_PLACEMENT_3D('',#19900,#16054,#16055);
#12697=AXIS2_PLACEMENT_3D('',#19901,#16056,#16057);
#12698=AXIS2_PLACEMENT_3D('',#19902,#16058,#16059);
#12699=AXIS2_PLACEMENT_3D('',#19903,#16060,#16061);
#12700=AXIS2_PLACEMENT_3D('',#19904,#16062,#16063);
#12701=AXIS2_PLACEMENT_3D('',#19905,#16064,#16065);
#12702=AXIS2_PLACEMENT_3D('',#19906,#16066,#16067);
#12703=AXIS2_PLACEMENT_3D('',#19907,#16068,#16069);
#12704=AXIS2_PLACEMENT_3D('',#19908,#16070,#16071);
#12705=AXIS2_PLACEMENT_3D('',#19909,#16072,#16073);
#12706=AXIS2_PLACEMENT_3D('',#19910,#16074,#16075);
#12707=AXIS2_PLACEMENT_3D('',#19911,#16076,#16077);
#12708=AXIS2_PLACEMENT_3D('',#19912,#16078,#16079);
#12709=AXIS2_PLACEMENT_3D('',#19913,#16080,#16081);
#12710=AXIS2_PLACEMENT_3D('',#19914,#16082,#16083);
#12711=AXIS2_PLACEMENT_3D('',#19915,#16084,#16085);
#12712=AXIS2_PLACEMENT_3D('',#19916,#16086,#16087);
#12713=AXIS2_PLACEMENT_3D('',#19917,#16088,#16089);
#12714=AXIS2_PLACEMENT_3D('',#19918,#16090,#16091);
#12715=AXIS2_PLACEMENT_3D('',#19919,#16092,#16093);
#12716=AXIS2_PLACEMENT_3D('',#19920,#16094,#16095);
#12717=AXIS2_PLACEMENT_3D('',#19921,#16096,#16097);
#12718=AXIS2_PLACEMENT_3D('',#19922,#16098,#16099);
#12719=AXIS2_PLACEMENT_3D('',#19923,#16100,#16101);
#12720=AXIS2_PLACEMENT_3D('',#19924,#16102,#16103);
#12721=AXIS2_PLACEMENT_3D('',#19925,#16104,#16105);
#12722=AXIS2_PLACEMENT_3D('',#19926,#16106,#16107);
#12723=AXIS2_PLACEMENT_3D('',#19927,#16108,#16109);
#12724=AXIS2_PLACEMENT_3D('',#19928,#16110,#16111);
#12725=AXIS2_PLACEMENT_3D('',#19929,#16112,#16113);
#12726=AXIS2_PLACEMENT_3D('',#19930,#16114,#16115);
#12727=AXIS2_PLACEMENT_3D('',#19931,#16116,#16117);
#12728=AXIS2_PLACEMENT_3D('',#19932,#16118,#16119);
#12729=AXIS2_PLACEMENT_3D('',#19933,#16120,#16121);
#12730=AXIS2_PLACEMENT_3D('',#19934,#16122,#16123);
#12731=AXIS2_PLACEMENT_3D('',#19935,#16124,#16125);
#12732=AXIS2_PLACEMENT_3D('',#19936,#16126,#16127);
#12733=AXIS2_PLACEMENT_3D('',#19937,#16128,#16129);
#12734=AXIS2_PLACEMENT_3D('',#19938,#16130,#16131);
#12735=AXIS2_PLACEMENT_3D('',#19939,#16132,#16133);
#12736=AXIS2_PLACEMENT_3D('',#19940,#16134,#16135);
#12737=AXIS2_PLACEMENT_3D('',#19941,#16136,#16137);
#12738=AXIS2_PLACEMENT_3D('',#19942,#16138,#16139);
#12739=AXIS2_PLACEMENT_3D('',#19943,#16140,#16141);
#12740=AXIS2_PLACEMENT_3D('',#19944,#16142,#16143);
#12741=AXIS2_PLACEMENT_3D('',#19945,#16144,#16145);
#12742=AXIS2_PLACEMENT_3D('',#19946,#16146,#16147);
#12743=AXIS2_PLACEMENT_3D('',#19947,#16148,#16149);
#12744=AXIS2_PLACEMENT_3D('',#19948,#16150,#16151);
#12745=AXIS2_PLACEMENT_3D('',#19949,#16152,#16153);
#12746=AXIS2_PLACEMENT_3D('',#19950,#16154,#16155);
#12747=AXIS2_PLACEMENT_3D('',#19951,#16156,#16157);
#12748=AXIS2_PLACEMENT_3D('',#19952,#16158,#16159);
#12749=AXIS2_PLACEMENT_3D('',#19953,#16160,#16161);
#12750=AXIS2_PLACEMENT_3D('',#19954,#16162,#16163);
#12751=AXIS2_PLACEMENT_3D('',#19955,#16164,#16165);
#12752=AXIS2_PLACEMENT_3D('',#19956,#16166,#16167);
#12753=AXIS2_PLACEMENT_3D('',#19957,#16168,#16169);
#12754=AXIS2_PLACEMENT_3D('',#19958,#16170,#16171);
#12755=AXIS2_PLACEMENT_3D('',#19959,#16172,#16173);
#12756=AXIS2_PLACEMENT_3D('',#19960,#16174,#16175);
#12757=AXIS2_PLACEMENT_3D('',#19961,#16176,#16177);
#12758=AXIS2_PLACEMENT_3D('',#19962,#16178,#16179);
#12759=AXIS2_PLACEMENT_3D('',#19963,#16180,#16181);
#12760=AXIS2_PLACEMENT_3D('',#19964,#16182,#16183);
#12761=AXIS2_PLACEMENT_3D('',#19965,#16184,#16185);
#12762=AXIS2_PLACEMENT_3D('',#19966,#16186,#16187);
#12763=AXIS2_PLACEMENT_3D('',#19967,#16188,#16189);
#12764=AXIS2_PLACEMENT_3D('',#19968,#16190,#16191);
#12765=AXIS2_PLACEMENT_3D('',#19969,#16192,#16193);
#12766=AXIS2_PLACEMENT_3D('',#19970,#16194,#16195);
#12767=AXIS2_PLACEMENT_3D('',#19971,#16196,#16197);
#12768=AXIS2_PLACEMENT_3D('',#19972,#16198,#16199);
#12769=AXIS2_PLACEMENT_3D('',#19973,#16200,#16201);
#12770=AXIS2_PLACEMENT_3D('',#19974,#16202,#16203);
#12771=AXIS2_PLACEMENT_3D('',#19975,#16204,#16205);
#12772=AXIS2_PLACEMENT_3D('',#19976,#16206,#16207);
#12773=AXIS2_PLACEMENT_3D('',#19977,#16208,#16209);
#12774=AXIS2_PLACEMENT_3D('',#19978,#16210,#16211);
#12775=AXIS2_PLACEMENT_3D('',#19979,#16212,#16213);
#12776=AXIS2_PLACEMENT_3D('',#19980,#16214,#16215);
#12777=AXIS2_PLACEMENT_3D('',#19981,#16216,#16217);
#12778=AXIS2_PLACEMENT_3D('',#19982,#16218,#16219);
#12779=AXIS2_PLACEMENT_3D('',#19983,#16220,#16221);
#12780=AXIS2_PLACEMENT_3D('',#19984,#16222,#16223);
#12781=AXIS2_PLACEMENT_3D('',#19985,#16224,#16225);
#12782=AXIS2_PLACEMENT_3D('',#19986,#16226,#16227);
#12783=AXIS2_PLACEMENT_3D('',#19987,#16228,#16229);
#12784=AXIS2_PLACEMENT_3D('',#19988,#16230,#16231);
#12785=DIRECTION('axis',(0.,0.,1.));
#12786=DIRECTION('refdir',(1.,0.,0.));
#12787=DIRECTION('axis',(0.,0.,1.));
#12788=DIRECTION('refdir',(1.,0.,0.));
#12789=DIRECTION('axis',(0.,0.,1.));
#12790=DIRECTION('refdir',(1.,0.,0.));
#12791=DIRECTION('center_axis',(0.,0.,1.));
#12792=DIRECTION('ref_axis',(1.,0.,0.));
#12793=DIRECTION('center_axis',(0.,0.,1.));
#12794=DIRECTION('ref_axis',(1.,0.,0.));
#12795=DIRECTION('',(0.,0.,1.));
#12796=DIRECTION('center_axis',(0.,0.,-1.));
#12797=DIRECTION('ref_axis',(1.,0.,0.));
#12798=DIRECTION('center_axis',(0.,0.,1.));
#12799=DIRECTION('ref_axis',(1.,0.,0.));
#12800=DIRECTION('center_axis',(0.,0.,1.));
#12801=DIRECTION('ref_axis',(1.,0.,0.));
#12802=DIRECTION('center_axis',(0.,0.,1.));
#12803=DIRECTION('ref_axis',(1.,0.,0.));
#12804=DIRECTION('',(0.,0.,1.));
#12805=DIRECTION('center_axis',(0.,0.,-1.));
#12806=DIRECTION('ref_axis',(1.,0.,0.));
#12807=DIRECTION('center_axis',(0.,0.,1.));
#12808=DIRECTION('ref_axis',(1.,0.,0.));
#12809=DIRECTION('center_axis',(0.,0.,1.));
#12810=DIRECTION('ref_axis',(1.,0.,0.));
#12811=DIRECTION('center_axis',(0.,0.,1.));
#12812=DIRECTION('ref_axis',(1.,0.,0.));
#12813=DIRECTION('',(0.,0.,1.));
#12814=DIRECTION('center_axis',(0.,0.,-1.));
#12815=DIRECTION('ref_axis',(1.,0.,0.));
#12816=DIRECTION('center_axis',(0.,0.,1.));
#12817=DIRECTION('ref_axis',(1.,0.,0.));
#12818=DIRECTION('center_axis',(0.,0.,1.));
#12819=DIRECTION('ref_axis',(1.,0.,0.));
#12820=DIRECTION('center_axis',(0.,0.,1.));
#12821=DIRECTION('ref_axis',(1.,0.,0.));
#12822=DIRECTION('',(0.,0.,1.));
#12823=DIRECTION('center_axis',(0.,0.,-1.));
#12824=DIRECTION('ref_axis',(1.,0.,0.));
#12825=DIRECTION('center_axis',(0.,0.,1.));
#12826=DIRECTION('ref_axis',(1.,0.,0.));
#12827=DIRECTION('center_axis',(0.,0.,1.));
#12828=DIRECTION('ref_axis',(1.,0.,0.));
#12829=DIRECTION('center_axis',(0.,0.,1.));
#12830=DIRECTION('ref_axis',(1.,0.,0.));
#12831=DIRECTION('',(0.,0.,1.));
#12832=DIRECTION('center_axis',(0.,0.,-1.));
#12833=DIRECTION('ref_axis',(1.,0.,0.));
#12834=DIRECTION('center_axis',(0.,0.,1.));
#12835=DIRECTION('ref_axis',(1.,0.,0.));
#12836=DIRECTION('center_axis',(0.,0.,1.));
#12837=DIRECTION('ref_axis',(1.,0.,0.));
#12838=DIRECTION('center_axis',(0.,0.,1.));
#12839=DIRECTION('ref_axis',(1.,0.,0.));
#12840=DIRECTION('',(0.,0.,1.));
#12841=DIRECTION('center_axis',(0.,0.,-1.));
#12842=DIRECTION('ref_axis',(1.,0.,0.));
#12843=DIRECTION('center_axis',(0.,0.,1.));
#12844=DIRECTION('ref_axis',(1.,0.,0.));
#12845=DIRECTION('center_axis',(0.,0.,1.));
#12846=DIRECTION('ref_axis',(1.,0.,0.));
#12847=DIRECTION('center_axis',(0.,0.,1.));
#12848=DIRECTION('ref_axis',(1.,0.,0.));
#12849=DIRECTION('',(0.,0.,1.));
#12850=DIRECTION('center_axis',(0.,0.,-1.));
#12851=DIRECTION('ref_axis',(1.,0.,0.));
#12852=DIRECTION('center_axis',(0.,0.,1.));
#12853=DIRECTION('ref_axis',(1.,0.,0.));
#12854=DIRECTION('center_axis',(0.,0.,1.));
#12855=DIRECTION('ref_axis',(1.,0.,0.));
#12856=DIRECTION('center_axis',(0.,0.,1.));
#12857=DIRECTION('ref_axis',(1.,0.,0.));
#12858=DIRECTION('',(0.,0.,1.));
#12859=DIRECTION('center_axis',(0.,0.,-1.));
#12860=DIRECTION('ref_axis',(1.,0.,0.));
#12861=DIRECTION('center_axis',(0.,0.,1.));
#12862=DIRECTION('ref_axis',(1.,0.,0.));
#12863=DIRECTION('center_axis',(0.,0.,1.));
#12864=DIRECTION('ref_axis',(1.,0.,0.));
#12865=DIRECTION('center_axis',(0.,0.,1.));
#12866=DIRECTION('ref_axis',(1.,0.,0.));
#12867=DIRECTION('',(0.,0.,1.));
#12868=DIRECTION('center_axis',(0.,0.,-1.));
#12869=DIRECTION('ref_axis',(1.,0.,0.));
#12870=DIRECTION('center_axis',(0.,0.,1.));
#12871=DIRECTION('ref_axis',(1.,0.,0.));
#12872=DIRECTION('center_axis',(0.,0.,1.));
#12873=DIRECTION('ref_axis',(1.,0.,0.));
#12874=DIRECTION('',(0.,0.,1.));
#12875=DIRECTION('center_axis',(0.,0.,-1.));
#12876=DIRECTION('ref_axis',(1.,0.,0.));
#12877=DIRECTION('center_axis',(0.,0.,1.));
#12878=DIRECTION('ref_axis',(1.,0.,0.));
#12879=DIRECTION('center_axis',(0.,0.,1.));
#12880=DIRECTION('ref_axis',(1.,0.,0.));
#12881=DIRECTION('',(0.,0.,1.));
#12882=DIRECTION('center_axis',(0.,0.,-1.));
#12883=DIRECTION('ref_axis',(1.,0.,0.));
#12884=DIRECTION('center_axis',(0.,0.,1.));
#12885=DIRECTION('ref_axis',(1.,0.,0.));
#12886=DIRECTION('center_axis',(0.,0.,1.));
#12887=DIRECTION('ref_axis',(1.,0.,0.));
#12888=DIRECTION('',(0.,0.,1.));
#12889=DIRECTION('center_axis',(0.,0.,-1.));
#12890=DIRECTION('ref_axis',(1.,0.,0.));
#12891=DIRECTION('center_axis',(0.,0.,1.));
#12892=DIRECTION('ref_axis',(1.,0.,0.));
#12893=DIRECTION('center_axis',(0.,0.,1.));
#12894=DIRECTION('ref_axis',(1.,0.,0.));
#12895=DIRECTION('',(0.,0.,1.));
#12896=DIRECTION('center_axis',(0.,0.,-1.));
#12897=DIRECTION('ref_axis',(1.,0.,0.));
#12898=DIRECTION('center_axis',(0.,0.,1.));
#12899=DIRECTION('ref_axis',(1.,0.,0.));
#12900=DIRECTION('center_axis',(0.,0.,1.));
#12901=DIRECTION('ref_axis',(1.,0.,0.));
#12902=DIRECTION('center_axis',(0.,0.,1.));
#12903=DIRECTION('ref_axis',(1.,0.,0.));
#12904=DIRECTION('',(0.,0.,1.));
#12905=DIRECTION('center_axis',(0.,0.,-1.));
#12906=DIRECTION('ref_axis',(1.,0.,0.));
#12907=DIRECTION('center_axis',(0.,0.,1.));
#12908=DIRECTION('ref_axis',(1.,0.,0.));
#12909=DIRECTION('center_axis',(0.,0.,1.));
#12910=DIRECTION('ref_axis',(1.,0.,0.));
#12911=DIRECTION('center_axis',(0.,0.,1.));
#12912=DIRECTION('ref_axis',(1.,0.,0.));
#12913=DIRECTION('',(0.,0.,1.));
#12914=DIRECTION('center_axis',(0.,0.,-1.));
#12915=DIRECTION('ref_axis',(1.,0.,0.));
#12916=DIRECTION('center_axis',(0.,0.,1.));
#12917=DIRECTION('ref_axis',(1.,0.,0.));
#12918=DIRECTION('center_axis',(0.,0.,1.));
#12919=DIRECTION('ref_axis',(1.,0.,0.));
#12920=DIRECTION('center_axis',(0.,0.,1.));
#12921=DIRECTION('ref_axis',(1.,0.,0.));
#12922=DIRECTION('',(0.,0.,1.));
#12923=DIRECTION('center_axis',(0.,0.,-1.));
#12924=DIRECTION('ref_axis',(1.,0.,0.));
#12925=DIRECTION('center_axis',(0.,0.,1.));
#12926=DIRECTION('ref_axis',(1.,0.,0.));
#12927=DIRECTION('center_axis',(0.,0.,1.));
#12928=DIRECTION('ref_axis',(1.,0.,0.));
#12929=DIRECTION('center_axis',(0.,0.,1.));
#12930=DIRECTION('ref_axis',(1.,0.,0.));
#12931=DIRECTION('',(0.,0.,1.));
#12932=DIRECTION('center_axis',(0.,0.,-1.));
#12933=DIRECTION('ref_axis',(1.,0.,0.));
#12934=DIRECTION('center_axis',(0.,0.,1.));
#12935=DIRECTION('ref_axis',(1.,0.,0.));
#12936=DIRECTION('center_axis',(0.,0.,1.));
#12937=DIRECTION('ref_axis',(1.,0.,0.));
#12938=DIRECTION('center_axis',(0.,0.,1.));
#12939=DIRECTION('ref_axis',(1.,0.,0.));
#12940=DIRECTION('',(0.,0.,1.));
#12941=DIRECTION('center_axis',(0.,0.,-1.));
#12942=DIRECTION('ref_axis',(1.,0.,0.));
#12943=DIRECTION('center_axis',(0.,0.,1.));
#12944=DIRECTION('ref_axis',(1.,0.,0.));
#12945=DIRECTION('center_axis',(0.,0.,1.));
#12946=DIRECTION('ref_axis',(1.,0.,0.));
#12947=DIRECTION('center_axis',(0.,0.,1.));
#12948=DIRECTION('ref_axis',(1.,0.,0.));
#12949=DIRECTION('',(0.,0.,1.));
#12950=DIRECTION('center_axis',(0.,0.,-1.));
#12951=DIRECTION('ref_axis',(1.,0.,0.));
#12952=DIRECTION('center_axis',(0.,0.,1.));
#12953=DIRECTION('ref_axis',(1.,0.,0.));
#12954=DIRECTION('center_axis',(0.,0.,1.));
#12955=DIRECTION('ref_axis',(1.,0.,0.));
#12956=DIRECTION('center_axis',(0.,0.,1.));
#12957=DIRECTION('ref_axis',(1.,0.,0.));
#12958=DIRECTION('',(0.,0.,1.));
#12959=DIRECTION('center_axis',(0.,0.,-1.));
#12960=DIRECTION('ref_axis',(1.,0.,0.));
#12961=DIRECTION('center_axis',(0.,0.,1.));
#12962=DIRECTION('ref_axis',(1.,0.,0.));
#12963=DIRECTION('center_axis',(0.,1.,0.));
#12964=DIRECTION('ref_axis',(-1.,0.,0.));
#12965=DIRECTION('',(-1.,0.,0.));
#12966=DIRECTION('',(0.,0.,1.));
#12967=DIRECTION('',(-1.,0.,0.));
#12968=DIRECTION('',(0.,0.,1.));
#12969=DIRECTION('center_axis',(1.,0.,0.));
#12970=DIRECTION('ref_axis',(0.,1.,0.));
#12971=DIRECTION('',(0.,1.,0.));
#12972=DIRECTION('',(0.,1.,0.));
#12973=DIRECTION('',(0.,0.,1.));
#12974=DIRECTION('center_axis',(0.,-1.,0.));
#12975=DIRECTION('ref_axis',(1.,0.,0.));
#12976=DIRECTION('',(1.,0.,0.));
#12977=DIRECTION('',(1.,0.,0.));
#12978=DIRECTION('',(0.,0.,1.));
#12979=DIRECTION('center_axis',(-1.,0.,0.));
#12980=DIRECTION('ref_axis',(0.,-1.,0.));
#12981=DIRECTION('',(0.,-1.,0.));
#12982=DIRECTION('',(0.,-1.,0.));
#12983=DIRECTION('center_axis',(0.,0.,1.));
#12984=DIRECTION('ref_axis',(1.,0.,0.));
#12985=DIRECTION('center_axis',(0.,0.,1.));
#12986=DIRECTION('ref_axis',(1.,0.,0.));
#12987=DIRECTION('axis',(0.,0.,1.));
#12988=DIRECTION('refdir',(1.,0.,0.));
#12989=DIRECTION('center_axis',(0.,-1.,0.));
#12990=DIRECTION('ref_axis',(1.,0.,0.));
#12991=DIRECTION('',(1.,0.,0.));
#12992=DIRECTION('',(0.,0.,-1.));
#12993=DIRECTION('',(-1.,0.,0.));
#12994=DIRECTION('',(0.,0.,1.));
#12995=DIRECTION('center_axis',(0.,0.,1.));
#12996=DIRECTION('ref_axis',(1.,0.,0.));
#12997=DIRECTION('',(0.,-1.,0.));
#12998=DIRECTION('',(1.,0.,0.));
#12999=DIRECTION('',(0.,1.,0.));
#13000=DIRECTION('center_axis',(-1.,0.,0.));
#13001=DIRECTION('ref_axis',(0.,-1.,0.));
#13002=DIRECTION('',(0.,-1.,0.));
#13003=DIRECTION('',(0.,0.,1.));
#13004=DIRECTION('center_axis',(0.,1.,0.));
#13005=DIRECTION('ref_axis',(-1.,0.,0.));
#13006=DIRECTION('',(-1.,0.,0.));
#13007=DIRECTION('',(0.,0.,-1.));
#13008=DIRECTION('center_axis',(0.,0.,1.));
#13009=DIRECTION('ref_axis',(1.,0.,0.));
#13010=DIRECTION('',(0.,1.,0.));
#13011=DIRECTION('center_axis',(1.,0.,0.));
#13012=DIRECTION('ref_axis',(0.,1.,0.));
#13013=DIRECTION('center_axis',(0.,-1.,0.));
#13014=DIRECTION('ref_axis',(1.,0.,0.));
#13015=DIRECTION('',(1.,0.,0.));
#13016=DIRECTION('',(0.,0.,1.));
#13017=DIRECTION('',(1.,0.,0.));
#13018=DIRECTION('',(0.,0.,1.));
#13019=DIRECTION('center_axis',(-1.,0.,0.));
#13020=DIRECTION('ref_axis',(0.,-1.,0.));
#13021=DIRECTION('',(0.,0.,-1.));
#13022=DIRECTION('',(0.,-1.,0.));
#13023=DIRECTION('',(0.,-1.,0.));
#13024=DIRECTION('center_axis',(0.,0.,1.));
#13025=DIRECTION('ref_axis',(1.,0.,0.));
#13026=DIRECTION('',(-1.,0.,0.));
#13027=DIRECTION('',(0.,1.,0.));
#13028=DIRECTION('center_axis',(1.,0.,0.));
#13029=DIRECTION('ref_axis',(0.,1.,0.));
#13030=DIRECTION('',(0.,0.,1.));
#13031=DIRECTION('',(0.,1.,0.));
#13032=DIRECTION('center_axis',(0.,0.,1.));
#13033=DIRECTION('ref_axis',(1.,0.,0.));
#13034=DIRECTION('',(1.,0.,0.));
#13035=DIRECTION('center_axis',(0.,-1.,0.));
#13036=DIRECTION('ref_axis',(1.,0.,0.));
#13037=DIRECTION('axis',(0.,0.,1.));
#13038=DIRECTION('refdir',(1.,0.,0.));
#13039=DIRECTION('center_axis',(0.,-1.,0.));
#13040=DIRECTION('ref_axis',(1.,0.,0.));
#13041=DIRECTION('',(1.,0.,0.));
#13042=DIRECTION('',(0.,0.,-1.));
#13043=DIRECTION('',(-1.,0.,0.));
#13044=DIRECTION('',(0.,0.,1.));
#13045=DIRECTION('center_axis',(0.,0.,1.));
#13046=DIRECTION('ref_axis',(1.,0.,0.));
#13047=DIRECTION('',(0.,-1.,0.));
#13048=DIRECTION('',(1.,0.,0.));
#13049=DIRECTION('',(0.,1.,0.));
#13050=DIRECTION('center_axis',(-1.,0.,0.));
#13051=DIRECTION('ref_axis',(0.,-1.,0.));
#13052=DIRECTION('',(0.,-1.,0.));
#13053=DIRECTION('',(0.,0.,1.));
#13054=DIRECTION('center_axis',(0.,1.,0.));
#13055=DIRECTION('ref_axis',(-1.,0.,0.));
#13056=DIRECTION('',(-1.,0.,0.));
#13057=DIRECTION('',(0.,0.,-1.));
#13058=DIRECTION('center_axis',(0.,0.,1.));
#13059=DIRECTION('ref_axis',(1.,0.,0.));
#13060=DIRECTION('',(0.,1.,0.));
#13061=DIRECTION('center_axis',(1.,0.,0.));
#13062=DIRECTION('ref_axis',(0.,1.,0.));
#13063=DIRECTION('center_axis',(0.,-1.,0.));
#13064=DIRECTION('ref_axis',(1.,0.,0.));
#13065=DIRECTION('',(1.,0.,0.));
#13066=DIRECTION('',(0.,0.,1.));
#13067=DIRECTION('',(1.,0.,0.));
#13068=DIRECTION('',(0.,0.,1.));
#13069=DIRECTION('center_axis',(-1.,0.,0.));
#13070=DIRECTION('ref_axis',(0.,-1.,0.));
#13071=DIRECTION('',(0.,0.,-1.));
#13072=DIRECTION('',(0.,-1.,0.));
#13073=DIRECTION('',(0.,-1.,0.));
#13074=DIRECTION('center_axis',(0.,0.,1.));
#13075=DIRECTION('ref_axis',(1.,0.,0.));
#13076=DIRECTION('',(-1.,0.,0.));
#13077=DIRECTION('',(0.,1.,0.));
#13078=DIRECTION('center_axis',(1.,0.,0.));
#13079=DIRECTION('ref_axis',(0.,1.,0.));
#13080=DIRECTION('',(0.,0.,1.));
#13081=DIRECTION('',(0.,1.,0.));
#13082=DIRECTION('center_axis',(0.,0.,1.));
#13083=DIRECTION('ref_axis',(1.,0.,0.));
#13084=DIRECTION('',(1.,0.,0.));
#13085=DIRECTION('center_axis',(0.,-1.,0.));
#13086=DIRECTION('ref_axis',(1.,0.,0.));
#13087=DIRECTION('axis',(0.,0.,1.));
#13088=DIRECTION('refdir',(1.,0.,0.));
#13089=DIRECTION('center_axis',(0.,1.,0.));
#13090=DIRECTION('ref_axis',(1.,0.,0.));
#13091=DIRECTION('center_axis',(0.,1.,0.));
#13092=DIRECTION('ref_axis',(1.,0.,0.));
#13093=DIRECTION('',(0.,1.,0.));
#13094=DIRECTION('center_axis',(0.,-1.,0.));
#13095=DIRECTION('ref_axis',(1.,0.,0.));
#13096=DIRECTION('center_axis',(0.,1.,0.));
#13097=DIRECTION('ref_axis',(1.,0.,0.));
#13098=DIRECTION('center_axis',(0.,1.,0.));
#13099=DIRECTION('ref_axis',(1.,0.,0.));
#13100=DIRECTION('',(0.,1.,0.));
#13101=DIRECTION('center_axis',(0.,-1.,0.));
#13102=DIRECTION('ref_axis',(1.,0.,0.));
#13103=DIRECTION('center_axis',(0.,1.,0.));
#13104=DIRECTION('ref_axis',(1.,0.,0.));
#13105=DIRECTION('center_axis',(0.,1.,0.));
#13106=DIRECTION('ref_axis',(1.,0.,0.));
#13107=DIRECTION('',(0.,1.,0.));
#13108=DIRECTION('center_axis',(0.,-1.,0.));
#13109=DIRECTION('ref_axis',(1.,0.,0.));
#13110=DIRECTION('center_axis',(0.,1.,0.));
#13111=DIRECTION('ref_axis',(1.,0.,0.));
#13112=DIRECTION('center_axis',(0.,1.,0.));
#13113=DIRECTION('ref_axis',(1.,0.,0.));
#13114=DIRECTION('',(0.,1.,0.));
#13115=DIRECTION('center_axis',(0.,-1.,0.));
#13116=DIRECTION('ref_axis',(1.,0.,0.));
#13117=DIRECTION('center_axis',(0.,1.,0.));
#13118=DIRECTION('ref_axis',(1.,0.,0.));
#13119=DIRECTION('center_axis',(0.,1.,0.));
#13120=DIRECTION('ref_axis',(1.,0.,0.));
#13121=DIRECTION('',(0.,1.,0.));
#13122=DIRECTION('center_axis',(0.,-1.,0.));
#13123=DIRECTION('ref_axis',(1.,0.,0.));
#13124=DIRECTION('center_axis',(0.,0.,1.));
#13125=DIRECTION('ref_axis',(1.,0.,0.));
#13126=DIRECTION('center_axis',(0.,0.,1.));
#13127=DIRECTION('ref_axis',(1.,0.,0.));
#13128=DIRECTION('',(0.,0.,1.));
#13129=DIRECTION('center_axis',(0.,0.,-1.));
#13130=DIRECTION('ref_axis',(1.,0.,0.));
#13131=DIRECTION('center_axis',(0.,0.,1.));
#13132=DIRECTION('ref_axis',(1.,0.,0.));
#13133=DIRECTION('center_axis',(0.,0.,1.));
#13134=DIRECTION('ref_axis',(1.,0.,0.));
#13135=DIRECTION('',(0.,0.,1.));
#13136=DIRECTION('center_axis',(0.,0.,-1.));
#13137=DIRECTION('ref_axis',(1.,0.,0.));
#13138=DIRECTION('center_axis',(0.,0.,1.));
#13139=DIRECTION('ref_axis',(1.,0.,0.));
#13140=DIRECTION('center_axis',(0.,0.,1.));
#13141=DIRECTION('ref_axis',(1.,0.,0.));
#13142=DIRECTION('',(0.,0.,1.));
#13143=DIRECTION('center_axis',(0.,0.,-1.));
#13144=DIRECTION('ref_axis',(1.,0.,0.));
#13145=DIRECTION('center_axis',(0.,0.,1.));
#13146=DIRECTION('ref_axis',(1.,0.,0.));
#13147=DIRECTION('center_axis',(0.,0.,1.));
#13148=DIRECTION('ref_axis',(1.,0.,0.));
#13149=DIRECTION('',(0.,0.,1.));
#13150=DIRECTION('center_axis',(0.,0.,-1.));
#13151=DIRECTION('ref_axis',(1.,0.,0.));
#13152=DIRECTION('center_axis',(0.,0.,1.));
#13153=DIRECTION('ref_axis',(1.,0.,0.));
#13154=DIRECTION('',(0.,1.,0.));
#13155=DIRECTION('',(-1.,0.,0.));
#13156=DIRECTION('',(0.,1.,0.));
#13157=DIRECTION('',(1.,0.,0.));
#13158=DIRECTION('center_axis',(0.,0.,1.));
#13159=DIRECTION('ref_axis',(1.,0.,0.));
#13160=DIRECTION('',(0.,-1.,0.));
#13161=DIRECTION('',(1.,0.,0.));
#13162=DIRECTION('',(0.,1.,0.));
#13163=DIRECTION('',(-1.,0.,0.));
#13164=DIRECTION('center_axis',(-1.,0.,0.));
#13165=DIRECTION('ref_axis',(0.,0.,1.));
#13166=DIRECTION('',(0.,0.,-1.));
#13167=DIRECTION('',(0.,0.,1.));
#13168=DIRECTION('',(0.,1.,0.));
#13169=DIRECTION('center_axis',(1.,0.,0.));
#13170=DIRECTION('ref_axis',(0.,0.,-1.));
#13171=DIRECTION('',(0.,0.,1.));
#13172=DIRECTION('',(0.,1.,0.));
#13173=DIRECTION('',(0.,0.,-1.));
#13174=DIRECTION('center_axis',(0.,-1.,0.));
#13175=DIRECTION('ref_axis',(1.,0.,0.));
#13176=DIRECTION('',(0.,0.,1.));
#13177=DIRECTION('',(1.,0.,0.));
#13178=DIRECTION('',(0.,0.,1.));
#13179=DIRECTION('',(1.,0.,0.));
#13180=DIRECTION('center_axis',(1.,0.,0.));
#13181=DIRECTION('ref_axis',(0.,1.,0.));
#13182=DIRECTION('',(0.,0.,1.));
#13183=DIRECTION('',(0.,1.,0.));
#13184=DIRECTION('center_axis',(0.,1.,0.));
#13185=DIRECTION('ref_axis',(-1.,0.,0.));
#13186=DIRECTION('',(0.,0.,1.));
#13187=DIRECTION('',(-1.,0.,0.));
#13188=DIRECTION('',(-1.,0.,0.));
#13189=DIRECTION('center_axis',(-1.,0.,0.));
#13190=DIRECTION('ref_axis',(0.,-1.,0.));
#13191=DIRECTION('',(0.,-1.,0.));
#13192=DIRECTION('center_axis',(0.,0.,1.));
#13193=DIRECTION('ref_axis',(1.,0.,0.));
#13194=DIRECTION('center_axis',(0.,0.,1.));
#13195=DIRECTION('ref_axis',(1.,0.,0.));
#13196=DIRECTION('axis',(0.,0.,1.));
#13197=DIRECTION('refdir',(1.,0.,0.));
#13198=DIRECTION('center_axis',(0.,1.,0.));
#13199=DIRECTION('ref_axis',(1.,0.,0.));
#13200=DIRECTION('center_axis',(0.,-1.,0.));
#13201=DIRECTION('ref_axis',(1.,0.,0.));
#13202=DIRECTION('',(0.,-1.,0.));
#13203=DIRECTION('center_axis',(0.,-1.,0.));
#13204=DIRECTION('ref_axis',(1.,0.,0.));
#13205=DIRECTION('center_axis',(0.,1.,0.));
#13206=DIRECTION('ref_axis',(1.,0.,0.));
#13207=DIRECTION('center_axis',(0.,1.,0.));
#13208=DIRECTION('ref_axis',(1.,0.,0.));
#13209=DIRECTION('',(0.,-1.,0.));
#13210=DIRECTION('center_axis',(0.,1.,0.));
#13211=DIRECTION('ref_axis',(1.,0.,0.));
#13212=DIRECTION('center_axis',(0.,1.,0.));
#13213=DIRECTION('ref_axis',(1.,0.,0.));
#13214=DIRECTION('center_axis',(0.,1.,0.));
#13215=DIRECTION('ref_axis',(1.,0.,0.));
#13216=DIRECTION('axis',(0.,0.,1.));
#13217=DIRECTION('refdir',(1.,0.,0.));
#13218=DIRECTION('center_axis',(0.,1.,0.));
#13219=DIRECTION('ref_axis',(0.707106781186546,0.,0.707106781186549));
#13220=DIRECTION('',(0.,1.,0.));
#13221=DIRECTION('center_axis',(0.,1.,0.));
#13222=DIRECTION('ref_axis',(1.,0.,0.));
#13223=DIRECTION('',(0.,-1.,0.));
#13224=DIRECTION('center_axis',(0.,-1.,0.));
#13225=DIRECTION('ref_axis',(1.,0.,0.));
#13226=DIRECTION('center_axis',(0.,1.,0.));
#13227=DIRECTION('ref_axis',(0.707106781186547,0.,-0.707106781186548));
#13228=DIRECTION('',(0.,1.,0.));
#13229=DIRECTION('center_axis',(0.,1.,0.));
#13230=DIRECTION('ref_axis',(1.,0.,0.));
#13231=DIRECTION('',(0.,-1.,0.));
#13232=DIRECTION('center_axis',(0.,-1.,0.));
#13233=DIRECTION('ref_axis',(1.,0.,0.));
#13234=DIRECTION('center_axis',(0.,1.,0.));
#13235=DIRECTION('ref_axis',(-0.707106781186552,0.,-0.707106781186543));
#13236=DIRECTION('',(0.,1.,0.));
#13237=DIRECTION('center_axis',(0.,1.,0.));
#13238=DIRECTION('ref_axis',(1.,0.,0.));
#13239=DIRECTION('',(0.,-1.,0.));
#13240=DIRECTION('center_axis',(0.,-1.,0.));
#13241=DIRECTION('ref_axis',(1.,0.,0.));
#13242=DIRECTION('center_axis',(0.,1.,0.));
#13243=DIRECTION('ref_axis',(-0.707106781186546,0.,0.707106781186549));
#13244=DIRECTION('',(0.,1.,0.));
#13245=DIRECTION('center_axis',(0.,1.,0.));
#13246=DIRECTION('ref_axis',(1.,0.,0.));
#13247=DIRECTION('',(0.,-1.,0.));
#13248=DIRECTION('center_axis',(0.,-1.,0.));
#13249=DIRECTION('ref_axis',(1.,0.,0.));
#13250=DIRECTION('center_axis',(0.,1.,0.));
#13251=DIRECTION('ref_axis',(1.,0.,0.));
#13252=DIRECTION('center_axis',(0.,1.,0.));
#13253=DIRECTION('ref_axis',(1.,0.,0.));
#13254=DIRECTION('center_axis',(0.,1.,0.));
#13255=DIRECTION('ref_axis',(1.,0.,0.));
#13256=DIRECTION('center_axis',(0.,1.,0.));
#13257=DIRECTION('ref_axis',(1.,0.,0.));
#13258=DIRECTION('center_axis',(0.,1.,0.));
#13259=DIRECTION('ref_axis',(1.,0.,0.));
#13260=DIRECTION('center_axis',(0.,-1.,0.));
#13261=DIRECTION('ref_axis',(1.,0.,0.));
#13262=DIRECTION('center_axis',(0.,1.,0.));
#13263=DIRECTION('ref_axis',(1.,0.,0.));
#13264=DIRECTION('center_axis',(0.,1.,0.));
#13265=DIRECTION('ref_axis',(1.,0.,0.));
#13266=DIRECTION('center_axis',(0.,1.,0.));
#13267=DIRECTION('ref_axis',(1.,0.,0.));
#13268=DIRECTION('center_axis',(0.,1.,0.));
#13269=DIRECTION('ref_axis',(1.,0.,0.));
#13270=DIRECTION('center_axis',(0.,1.,0.));
#13271=DIRECTION('ref_axis',(1.,0.,0.));
#13272=DIRECTION('center_axis',(0.,1.,0.));
#13273=DIRECTION('ref_axis',(1.,0.,0.));
#13274=DIRECTION('center_axis',(0.,1.,0.));
#13275=DIRECTION('ref_axis',(-1.,0.,-1.22464679914735E-16));
#13276=DIRECTION('center_axis',(0.,1.,0.));
#13277=DIRECTION('ref_axis',(1.,0.,0.));
#13278=DIRECTION('center_axis',(0.,1.,0.));
#13279=DIRECTION('ref_axis',(1.,0.,0.));
#13280=DIRECTION('center_axis',(0.,1.,0.));
#13281=DIRECTION('ref_axis',(1.,0.,0.));
#13282=DIRECTION('',(0.,-1.,0.));
#13283=DIRECTION('center_axis',(0.,-1.,0.));
#13284=DIRECTION('ref_axis',(1.,0.,0.));
#13285=DIRECTION('center_axis',(0.,1.,0.));
#13286=DIRECTION('ref_axis',(1.,0.,0.));
#13287=DIRECTION('center_axis',(0.,-1.,0.));
#13288=DIRECTION('ref_axis',(1.,0.,0.));
#13289=DIRECTION('center_axis',(0.,1.,0.));
#13290=DIRECTION('ref_axis',(1.,0.,0.));
#13291=DIRECTION('',(0.,-1.,0.));
#13292=DIRECTION('center_axis',(0.,1.,0.));
#13293=DIRECTION('ref_axis',(1.,0.,0.));
#13294=DIRECTION('axis',(0.,0.,1.));
#13295=DIRECTION('refdir',(1.,0.,0.));
#13296=DIRECTION('center_axis',(0.,1.,0.));
#13297=DIRECTION('ref_axis',(0.707106781186546,0.,0.707106781186549));
#13298=DIRECTION('',(0.,1.,0.));
#13299=DIRECTION('center_axis',(0.,1.,0.));
#13300=DIRECTION('ref_axis',(1.,0.,0.));
#13301=DIRECTION('',(0.,-1.,0.));
#13302=DIRECTION('center_axis',(0.,-1.,0.));
#13303=DIRECTION('ref_axis',(1.,0.,0.));
#13304=DIRECTION('center_axis',(0.,1.,0.));
#13305=DIRECTION('ref_axis',(0.707106781186547,0.,-0.707106781186548));
#13306=DIRECTION('',(0.,1.,0.));
#13307=DIRECTION('center_axis',(0.,1.,0.));
#13308=DIRECTION('ref_axis',(1.,0.,0.));
#13309=DIRECTION('',(0.,-1.,0.));
#13310=DIRECTION('center_axis',(0.,-1.,0.));
#13311=DIRECTION('ref_axis',(1.,0.,0.));
#13312=DIRECTION('center_axis',(0.,1.,0.));
#13313=DIRECTION('ref_axis',(-0.707106781186552,0.,-0.707106781186543));
#13314=DIRECTION('',(0.,1.,0.));
#13315=DIRECTION('center_axis',(0.,1.,0.));
#13316=DIRECTION('ref_axis',(1.,0.,0.));
#13317=DIRECTION('',(0.,-1.,0.));
#13318=DIRECTION('center_axis',(0.,-1.,0.));
#13319=DIRECTION('ref_axis',(1.,0.,0.));
#13320=DIRECTION('center_axis',(0.,1.,0.));
#13321=DIRECTION('ref_axis',(-0.707106781186546,0.,0.707106781186549));
#13322=DIRECTION('',(0.,1.,0.));
#13323=DIRECTION('center_axis',(0.,1.,0.));
#13324=DIRECTION('ref_axis',(1.,0.,0.));
#13325=DIRECTION('',(0.,-1.,0.));
#13326=DIRECTION('center_axis',(0.,-1.,0.));
#13327=DIRECTION('ref_axis',(1.,0.,0.));
#13328=DIRECTION('center_axis',(0.,1.,0.));
#13329=DIRECTION('ref_axis',(1.,0.,0.));
#13330=DIRECTION('center_axis',(0.,1.,0.));
#13331=DIRECTION('ref_axis',(1.,0.,0.));
#13332=DIRECTION('center_axis',(0.,1.,0.));
#13333=DIRECTION('ref_axis',(1.,0.,0.));
#13334=DIRECTION('center_axis',(0.,1.,0.));
#13335=DIRECTION('ref_axis',(1.,0.,0.));
#13336=DIRECTION('center_axis',(0.,1.,0.));
#13337=DIRECTION('ref_axis',(1.,0.,0.));
#13338=DIRECTION('center_axis',(0.,1.,0.));
#13339=DIRECTION('ref_axis',(1.,0.,0.));
#13340=DIRECTION('center_axis',(0.,1.,0.));
#13341=DIRECTION('ref_axis',(1.,0.,0.));
#13342=DIRECTION('center_axis',(0.,1.,0.));
#13343=DIRECTION('ref_axis',(1.,0.,0.));
#13344=DIRECTION('center_axis',(0.,1.,0.));
#13345=DIRECTION('ref_axis',(1.,0.,0.));
#13346=DIRECTION('center_axis',(0.,1.,0.));
#13347=DIRECTION('ref_axis',(1.,0.,0.));
#13348=DIRECTION('center_axis',(0.,1.,0.));
#13349=DIRECTION('ref_axis',(1.,0.,0.));
#13350=DIRECTION('center_axis',(0.,1.,0.));
#13351=DIRECTION('ref_axis',(1.,0.,0.));
#13352=DIRECTION('center_axis',(0.,1.,0.));
#13353=DIRECTION('ref_axis',(-1.,0.,-1.22464679914735E-16));
#13354=DIRECTION('center_axis',(0.,1.,0.));
#13355=DIRECTION('ref_axis',(1.,0.,0.));
#13356=DIRECTION('center_axis',(0.,1.,0.));
#13357=DIRECTION('ref_axis',(1.,0.,0.));
#13358=DIRECTION('',(0.,-1.,0.));
#13359=DIRECTION('center_axis',(0.,1.,0.));
#13360=DIRECTION('ref_axis',(1.,0.,0.));
#13361=DIRECTION('center_axis',(0.,1.,0.));
#13362=DIRECTION('ref_axis',(1.,0.,0.));
#13363=DIRECTION('center_axis',(0.,-1.,0.));
#13364=DIRECTION('ref_axis',(1.,0.,0.));
#13365=DIRECTION('center_axis',(0.,1.,0.));
#13366=DIRECTION('ref_axis',(1.,0.,0.));
#13367=DIRECTION('center_axis',(0.,-1.,0.));
#13368=DIRECTION('ref_axis',(1.,0.,0.));
#13369=DIRECTION('',(0.,-1.,0.));
#13370=DIRECTION('center_axis',(0.,1.,0.));
#13371=DIRECTION('ref_axis',(1.,0.,0.));
#13372=DIRECTION('axis',(0.,0.,1.));
#13373=DIRECTION('refdir',(1.,0.,0.));
#13374=DIRECTION('center_axis',(0.,1.,0.));
#13375=DIRECTION('ref_axis',(1.,0.,0.));
#13376=DIRECTION('center_axis',(0.,1.,0.));
#13377=DIRECTION('ref_axis',(1.,0.,0.));
#13378=DIRECTION('',(0.,1.,0.));
#13379=DIRECTION('center_axis',(0.,-1.,0.));
#13380=DIRECTION('ref_axis',(1.,0.,0.));
#13381=DIRECTION('center_axis',(0.,1.,0.));
#13382=DIRECTION('ref_axis',(1.,0.,0.));
#13383=DIRECTION('center_axis',(0.,1.,0.));
#13384=DIRECTION('ref_axis',(1.,0.,0.));
#13385=DIRECTION('',(0.,1.,0.));
#13386=DIRECTION('center_axis',(0.,-1.,0.));
#13387=DIRECTION('ref_axis',(1.,0.,0.));
#13388=DIRECTION('center_axis',(0.,1.,0.));
#13389=DIRECTION('ref_axis',(1.,0.,0.));
#13390=DIRECTION('center_axis',(0.,1.,0.));
#13391=DIRECTION('ref_axis',(1.,0.,0.));
#13392=DIRECTION('',(0.,1.,0.));
#13393=DIRECTION('center_axis',(0.,-1.,0.));
#13394=DIRECTION('ref_axis',(1.,0.,0.));
#13395=DIRECTION('center_axis',(0.,1.,0.));
#13396=DIRECTION('ref_axis',(1.,0.,0.));
#13397=DIRECTION('center_axis',(0.,1.,0.));
#13398=DIRECTION('ref_axis',(1.,0.,0.));
#13399=DIRECTION('',(0.,1.,0.));
#13400=DIRECTION('center_axis',(0.,-1.,0.));
#13401=DIRECTION('ref_axis',(1.,0.,0.));
#13402=DIRECTION('center_axis',(0.,1.,0.));
#13403=DIRECTION('ref_axis',(1.,0.,0.));
#13404=DIRECTION('center_axis',(0.,1.,0.));
#13405=DIRECTION('ref_axis',(1.,0.,0.));
#13406=DIRECTION('',(0.,1.,0.));
#13407=DIRECTION('center_axis',(0.,-1.,0.));
#13408=DIRECTION('ref_axis',(1.,0.,0.));
#13409=DIRECTION('center_axis',(0.,0.,1.));
#13410=DIRECTION('ref_axis',(1.,0.,0.));
#13411=DIRECTION('center_axis',(0.,0.,1.));
#13412=DIRECTION('ref_axis',(1.,0.,0.));
#13413=DIRECTION('',(0.,0.,1.));
#13414=DIRECTION('center_axis',(0.,0.,-1.));
#13415=DIRECTION('ref_axis',(1.,0.,0.));
#13416=DIRECTION('center_axis',(0.,0.,1.));
#13417=DIRECTION('ref_axis',(1.,0.,0.));
#13418=DIRECTION('center_axis',(0.,0.,1.));
#13419=DIRECTION('ref_axis',(1.,0.,0.));
#13420=DIRECTION('',(0.,0.,1.));
#13421=DIRECTION('center_axis',(0.,0.,-1.));
#13422=DIRECTION('ref_axis',(1.,0.,0.));
#13423=DIRECTION('center_axis',(0.,0.,1.));
#13424=DIRECTION('ref_axis',(1.,0.,0.));
#13425=DIRECTION('center_axis',(0.,0.,1.));
#13426=DIRECTION('ref_axis',(1.,0.,0.));
#13427=DIRECTION('',(0.,0.,1.));
#13428=DIRECTION('center_axis',(0.,0.,-1.));
#13429=DIRECTION('ref_axis',(1.,0.,0.));
#13430=DIRECTION('center_axis',(0.,0.,1.));
#13431=DIRECTION('ref_axis',(1.,0.,0.));
#13432=DIRECTION('center_axis',(0.,0.,1.));
#13433=DIRECTION('ref_axis',(1.,0.,0.));
#13434=DIRECTION('',(0.,0.,1.));
#13435=DIRECTION('center_axis',(0.,0.,-1.));
#13436=DIRECTION('ref_axis',(1.,0.,0.));
#13437=DIRECTION('center_axis',(0.,0.,1.));
#13438=DIRECTION('ref_axis',(1.,0.,0.));
#13439=DIRECTION('',(0.,1.,0.));
#13440=DIRECTION('',(-1.,0.,0.));
#13441=DIRECTION('',(0.,1.,0.));
#13442=DIRECTION('',(1.,0.,0.));
#13443=DIRECTION('center_axis',(0.,0.,1.));
#13444=DIRECTION('ref_axis',(1.,0.,0.));
#13445=DIRECTION('',(0.,-1.,0.));
#13446=DIRECTION('',(1.,0.,0.));
#13447=DIRECTION('',(0.,1.,0.));
#13448=DIRECTION('',(-1.,0.,0.));
#13449=DIRECTION('center_axis',(-1.,0.,0.));
#13450=DIRECTION('ref_axis',(0.,0.,1.));
#13451=DIRECTION('',(0.,0.,-1.));
#13452=DIRECTION('',(0.,0.,1.));
#13453=DIRECTION('',(0.,1.,0.));
#13454=DIRECTION('center_axis',(1.,0.,0.));
#13455=DIRECTION('ref_axis',(0.,0.,-1.));
#13456=DIRECTION('',(0.,0.,1.));
#13457=DIRECTION('',(0.,1.,0.));
#13458=DIRECTION('',(0.,0.,-1.));
#13459=DIRECTION('center_axis',(0.,-1.,0.));
#13460=DIRECTION('ref_axis',(1.,0.,0.));
#13461=DIRECTION('',(0.,0.,1.));
#13462=DIRECTION('',(1.,0.,0.));
#13463=DIRECTION('',(0.,0.,1.));
#13464=DIRECTION('',(1.,0.,0.));
#13465=DIRECTION('center_axis',(1.,0.,0.));
#13466=DIRECTION('ref_axis',(0.,1.,0.));
#13467=DIRECTION('',(0.,0.,1.));
#13468=DIRECTION('',(0.,1.,0.));
#13469=DIRECTION('center_axis',(0.,1.,0.));
#13470=DIRECTION('ref_axis',(-1.,0.,0.));
#13471=DIRECTION('',(0.,0.,1.));
#13472=DIRECTION('',(-1.,0.,0.));
#13473=DIRECTION('',(-1.,0.,0.));
#13474=DIRECTION('center_axis',(-1.,0.,0.));
#13475=DIRECTION('ref_axis',(0.,-1.,0.));
#13476=DIRECTION('',(0.,-1.,0.));
#13477=DIRECTION('center_axis',(0.,0.,1.));
#13478=DIRECTION('ref_axis',(1.,0.,0.));
#13479=DIRECTION('center_axis',(0.,0.,1.));
#13480=DIRECTION('ref_axis',(1.,0.,0.));
#13481=DIRECTION('axis',(0.,0.,1.));
#13482=DIRECTION('refdir',(1.,0.,0.));
#13483=DIRECTION('center_axis',(0.,1.,0.));
#13484=DIRECTION('ref_axis',(1.,0.,0.));
#13485=DIRECTION('center_axis',(0.,-1.,0.));
#13486=DIRECTION('ref_axis',(1.,0.,0.));
#13487=DIRECTION('',(0.,-1.,0.));
#13488=DIRECTION('center_axis',(0.,-1.,0.));
#13489=DIRECTION('ref_axis',(1.,0.,0.));
#13490=DIRECTION('center_axis',(0.,1.,0.));
#13491=DIRECTION('ref_axis',(1.,0.,0.));
#13492=DIRECTION('center_axis',(0.,1.,0.));
#13493=DIRECTION('ref_axis',(1.,0.,0.));
#13494=DIRECTION('',(0.,-1.,0.));
#13495=DIRECTION('center_axis',(0.,1.,0.));
#13496=DIRECTION('ref_axis',(1.,0.,0.));
#13497=DIRECTION('center_axis',(0.,1.,0.));
#13498=DIRECTION('ref_axis',(1.,0.,0.));
#13499=DIRECTION('center_axis',(0.,1.,0.));
#13500=DIRECTION('ref_axis',(1.,0.,0.));
#13501=DIRECTION('axis',(0.,0.,1.));
#13502=DIRECTION('refdir',(1.,0.,0.));
#13503=DIRECTION('center_axis',(0.,1.,0.));
#13504=DIRECTION('ref_axis',(0.70710678118656,0.,0.707106781186535));
#13505=DIRECTION('',(0.,1.,0.));
#13506=DIRECTION('center_axis',(0.,1.,0.));
#13507=DIRECTION('ref_axis',(1.,0.,0.));
#13508=DIRECTION('',(0.,-1.,0.));
#13509=DIRECTION('center_axis',(0.,-1.,0.));
#13510=DIRECTION('ref_axis',(1.,0.,0.));
#13511=DIRECTION('center_axis',(0.,1.,0.));
#13512=DIRECTION('ref_axis',(0.707106781186561,0.,-0.707106781186534));
#13513=DIRECTION('',(0.,1.,0.));
#13514=DIRECTION('center_axis',(0.,1.,0.));
#13515=DIRECTION('ref_axis',(1.,0.,0.));
#13516=DIRECTION('',(0.,-1.,0.));
#13517=DIRECTION('center_axis',(0.,-1.,0.));
#13518=DIRECTION('ref_axis',(1.,0.,0.));
#13519=DIRECTION('center_axis',(0.,1.,0.));
#13520=DIRECTION('ref_axis',(-0.707106781186554,0.,-0.707106781186541));
#13521=DIRECTION('',(0.,1.,0.));
#13522=DIRECTION('center_axis',(0.,1.,0.));
#13523=DIRECTION('ref_axis',(1.,0.,0.));
#13524=DIRECTION('',(0.,-1.,0.));
#13525=DIRECTION('center_axis',(0.,-1.,0.));
#13526=DIRECTION('ref_axis',(1.,0.,0.));
#13527=DIRECTION('center_axis',(0.,1.,0.));
#13528=DIRECTION('ref_axis',(-0.707106781186554,0.,0.707106781186541));
#13529=DIRECTION('',(0.,1.,0.));
#13530=DIRECTION('center_axis',(0.,1.,0.));
#13531=DIRECTION('ref_axis',(1.,0.,0.));
#13532=DIRECTION('',(0.,-1.,0.));
#13533=DIRECTION('center_axis',(0.,-1.,0.));
#13534=DIRECTION('ref_axis',(1.,0.,0.));
#13535=DIRECTION('center_axis',(0.,1.,0.));
#13536=DIRECTION('ref_axis',(1.,0.,0.));
#13537=DIRECTION('center_axis',(0.,1.,0.));
#13538=DIRECTION('ref_axis',(1.,0.,0.));
#13539=DIRECTION('center_axis',(0.,1.,0.));
#13540=DIRECTION('ref_axis',(1.,0.,0.));
#13541=DIRECTION('center_axis',(0.,1.,0.));
#13542=DIRECTION('ref_axis',(1.,0.,0.));
#13543=DIRECTION('center_axis',(0.,1.,0.));
#13544=DIRECTION('ref_axis',(1.,0.,0.));
#13545=DIRECTION('center_axis',(0.,-1.,0.));
#13546=DIRECTION('ref_axis',(1.,0.,0.));
#13547=DIRECTION('center_axis',(0.,1.,0.));
#13548=DIRECTION('ref_axis',(1.,0.,0.));
#13549=DIRECTION('center_axis',(0.,1.,0.));
#13550=DIRECTION('ref_axis',(1.,0.,0.));
#13551=DIRECTION('center_axis',(0.,1.,0.));
#13552=DIRECTION('ref_axis',(1.,0.,0.));
#13553=DIRECTION('center_axis',(0.,1.,0.));
#13554=DIRECTION('ref_axis',(1.,0.,0.));
#13555=DIRECTION('center_axis',(0.,1.,0.));
#13556=DIRECTION('ref_axis',(1.,0.,0.));
#13557=DIRECTION('center_axis',(0.,1.,0.));
#13558=DIRECTION('ref_axis',(1.,0.,0.));
#13559=DIRECTION('center_axis',(0.,1.,0.));
#13560=DIRECTION('ref_axis',(-1.,0.,-1.22464679914735E-16));
#13561=DIRECTION('center_axis',(0.,1.,0.));
#13562=DIRECTION('ref_axis',(1.,0.,0.));
#13563=DIRECTION('center_axis',(0.,1.,0.));
#13564=DIRECTION('ref_axis',(1.,0.,0.));
#13565=DIRECTION('center_axis',(0.,1.,0.));
#13566=DIRECTION('ref_axis',(1.,0.,0.));
#13567=DIRECTION('',(0.,-1.,0.));
#13568=DIRECTION('center_axis',(0.,-1.,0.));
#13569=DIRECTION('ref_axis',(1.,0.,0.));
#13570=DIRECTION('center_axis',(0.,1.,0.));
#13571=DIRECTION('ref_axis',(1.,0.,0.));
#13572=DIRECTION('center_axis',(0.,-1.,0.));
#13573=DIRECTION('ref_axis',(1.,0.,0.));
#13574=DIRECTION('center_axis',(0.,1.,0.));
#13575=DIRECTION('ref_axis',(1.,0.,0.));
#13576=DIRECTION('',(0.,-1.,0.));
#13577=DIRECTION('center_axis',(0.,1.,0.));
#13578=DIRECTION('ref_axis',(1.,0.,0.));
#13579=DIRECTION('axis',(0.,0.,1.));
#13580=DIRECTION('refdir',(1.,0.,0.));
#13581=DIRECTION('center_axis',(0.,1.,0.));
#13582=DIRECTION('ref_axis',(0.70710678118656,0.,0.707106781186535));
#13583=DIRECTION('',(0.,1.,0.));
#13584=DIRECTION('center_axis',(0.,1.,0.));
#13585=DIRECTION('ref_axis',(1.,0.,0.));
#13586=DIRECTION('',(0.,-1.,0.));
#13587=DIRECTION('center_axis',(0.,-1.,0.));
#13588=DIRECTION('ref_axis',(1.,0.,0.));
#13589=DIRECTION('center_axis',(0.,1.,0.));
#13590=DIRECTION('ref_axis',(0.707106781186561,0.,-0.707106781186534));
#13591=DIRECTION('',(0.,1.,0.));
#13592=DIRECTION('center_axis',(0.,1.,0.));
#13593=DIRECTION('ref_axis',(1.,0.,0.));
#13594=DIRECTION('',(0.,-1.,0.));
#13595=DIRECTION('center_axis',(0.,-1.,0.));
#13596=DIRECTION('ref_axis',(1.,0.,0.));
#13597=DIRECTION('center_axis',(0.,1.,0.));
#13598=DIRECTION('ref_axis',(-0.707106781186554,0.,-0.707106781186541));
#13599=DIRECTION('',(0.,1.,0.));
#13600=DIRECTION('center_axis',(0.,1.,0.));
#13601=DIRECTION('ref_axis',(1.,0.,0.));
#13602=DIRECTION('',(0.,-1.,0.));
#13603=DIRECTION('center_axis',(0.,-1.,0.));
#13604=DIRECTION('ref_axis',(1.,0.,0.));
#13605=DIRECTION('center_axis',(0.,1.,0.));
#13606=DIRECTION('ref_axis',(-0.707106781186554,0.,0.707106781186541));
#13607=DIRECTION('',(0.,1.,0.));
#13608=DIRECTION('center_axis',(0.,1.,0.));
#13609=DIRECTION('ref_axis',(1.,0.,0.));
#13610=DIRECTION('',(0.,-1.,0.));
#13611=DIRECTION('center_axis',(0.,-1.,0.));
#13612=DIRECTION('ref_axis',(1.,0.,0.));
#13613=DIRECTION('center_axis',(0.,1.,0.));
#13614=DIRECTION('ref_axis',(1.,0.,0.));
#13615=DIRECTION('center_axis',(0.,1.,0.));
#13616=DIRECTION('ref_axis',(1.,0.,0.));
#13617=DIRECTION('center_axis',(0.,1.,0.));
#13618=DIRECTION('ref_axis',(1.,0.,0.));
#13619=DIRECTION('center_axis',(0.,1.,0.));
#13620=DIRECTION('ref_axis',(1.,0.,0.));
#13621=DIRECTION('center_axis',(0.,1.,0.));
#13622=DIRECTION('ref_axis',(1.,0.,0.));
#13623=DIRECTION('center_axis',(0.,1.,0.));
#13624=DIRECTION('ref_axis',(1.,0.,0.));
#13625=DIRECTION('center_axis',(0.,1.,0.));
#13626=DIRECTION('ref_axis',(1.,0.,0.));
#13627=DIRECTION('center_axis',(0.,1.,0.));
#13628=DIRECTION('ref_axis',(1.,0.,0.));
#13629=DIRECTION('center_axis',(0.,1.,0.));
#13630=DIRECTION('ref_axis',(1.,0.,0.));
#13631=DIRECTION('center_axis',(0.,1.,0.));
#13632=DIRECTION('ref_axis',(1.,0.,0.));
#13633=DIRECTION('center_axis',(0.,1.,0.));
#13634=DIRECTION('ref_axis',(1.,0.,0.));
#13635=DIRECTION('center_axis',(0.,1.,0.));
#13636=DIRECTION('ref_axis',(1.,0.,0.));
#13637=DIRECTION('center_axis',(0.,1.,0.));
#13638=DIRECTION('ref_axis',(-1.,0.,-1.22464679914735E-16));
#13639=DIRECTION('center_axis',(0.,1.,0.));
#13640=DIRECTION('ref_axis',(1.,0.,0.));
#13641=DIRECTION('center_axis',(0.,1.,0.));
#13642=DIRECTION('ref_axis',(1.,0.,0.));
#13643=DIRECTION('',(0.,-1.,0.));
#13644=DIRECTION('center_axis',(0.,1.,0.));
#13645=DIRECTION('ref_axis',(1.,0.,0.));
#13646=DIRECTION('center_axis',(0.,1.,0.));
#13647=DIRECTION('ref_axis',(1.,0.,0.));
#13648=DIRECTION('center_axis',(0.,-1.,0.));
#13649=DIRECTION('ref_axis',(1.,0.,0.));
#13650=DIRECTION('center_axis',(0.,1.,0.));
#13651=DIRECTION('ref_axis',(1.,0.,0.));
#13652=DIRECTION('center_axis',(0.,-1.,0.));
#13653=DIRECTION('ref_axis',(1.,0.,0.));
#13654=DIRECTION('',(0.,-1.,0.));
#13655=DIRECTION('center_axis',(0.,1.,0.));
#13656=DIRECTION('ref_axis',(1.,0.,0.));
#13657=DIRECTION('axis',(0.,0.,1.));
#13658=DIRECTION('refdir',(1.,0.,0.));
#13659=DIRECTION('center_axis',(0.,0.,-1.));
#13660=DIRECTION('ref_axis',(-1.,0.,0.));
#13661=DIRECTION('',(-1.,0.,0.));
#13662=DIRECTION('',(0.,-1.,0.));
#13663=DIRECTION('',(1.,0.,0.));
#13664=DIRECTION('',(0.,-1.,0.));
#13665=DIRECTION('center_axis',(0.,0.,1.));
#13666=DIRECTION('ref_axis',(1.,0.,0.));
#13667=DIRECTION('',(1.,0.,0.));
#13668=DIRECTION('',(0.,-1.,0.));
#13669=DIRECTION('',(-1.,0.,0.));
#13670=DIRECTION('',(0.,1.,0.));
#13671=DIRECTION('center_axis',(0.,1.,0.));
#13672=DIRECTION('ref_axis',(1.,0.,0.));
#13673=DIRECTION('',(1.,0.,0.));
#13674=DIRECTION('center_axis',(0.,1.,0.));
#13675=DIRECTION('ref_axis',(1.,0.,0.));
#13676=DIRECTION('',(-1.,0.,0.));
#13677=DIRECTION('center_axis',(0.,1.,0.));
#13678=DIRECTION('ref_axis',(1.,0.,0.));
#13679=DIRECTION('center_axis',(0.,1.,0.));
#13680=DIRECTION('ref_axis',(1.,0.,0.));
#13681=DIRECTION('center_axis',(0.,1.,0.));
#13682=DIRECTION('ref_axis',(1.,0.,0.));
#13683=DIRECTION('center_axis',(0.,1.,0.));
#13684=DIRECTION('ref_axis',(-1.,0.,-1.22464679914735E-16));
#13685=DIRECTION('center_axis',(0.,-1.,0.));
#13686=DIRECTION('ref_axis',(1.,0.,0.));
#13687=DIRECTION('center_axis',(0.,1.,0.));
#13688=DIRECTION('ref_axis',(1.,0.,0.));
#13689=DIRECTION('center_axis',(0.,-1.,0.));
#13690=DIRECTION('ref_axis',(1.,0.,0.));
#13691=DIRECTION('center_axis',(0.,1.,0.));
#13692=DIRECTION('ref_axis',(1.,0.,0.));
#13693=DIRECTION('',(0.,1.,0.));
#13694=DIRECTION('center_axis',(0.,1.,0.));
#13695=DIRECTION('ref_axis',(1.,0.,0.));
#13696=DIRECTION('',(0.,1.,0.));
#13697=DIRECTION('center_axis',(0.,0.,-1.));
#13698=DIRECTION('ref_axis',(-1.,0.,0.));
#13699=DIRECTION('',(0.,1.,0.));
#13700=DIRECTION('',(-1.,0.,0.));
#13701=DIRECTION('center_axis',(0.,0.,1.));
#13702=DIRECTION('ref_axis',(1.,0.,0.));
#13703=DIRECTION('',(1.,0.,0.));
#13704=DIRECTION('',(0.,1.,0.));
#13705=DIRECTION('center_axis',(0.,1.,0.));
#13706=DIRECTION('ref_axis',(-1.,0.,-1.22464679914735E-16));
#13707=DIRECTION('center_axis',(0.,1.,0.));
#13708=DIRECTION('ref_axis',(1.,0.,0.));
#13709=DIRECTION('center_axis',(0.,1.,0.));
#13710=DIRECTION('ref_axis',(1.,0.,0.));
#13711=DIRECTION('axis',(0.,0.,1.));
#13712=DIRECTION('refdir',(1.,0.,0.));
#13713=DIRECTION('center_axis',(0.,0.,1.));
#13714=DIRECTION('ref_axis',(1.,0.,0.));
#13715=DIRECTION('',(0.,0.,-1.));
#13716=DIRECTION('center_axis',(0.,0.,-1.));
#13717=DIRECTION('ref_axis',(1.,0.,0.));
#13718=DIRECTION('',(0.,0.,1.));
#13719=DIRECTION('center_axis',(0.,0.,1.));
#13720=DIRECTION('ref_axis',(1.,0.,0.));
#13721=DIRECTION('center_axis',(0.,0.,1.));
#13722=DIRECTION('ref_axis',(1.,0.,0.));
#13723=DIRECTION('',(0.,0.,1.));
#13724=DIRECTION('center_axis',(0.,0.,1.));
#13725=DIRECTION('ref_axis',(1.,0.,0.));
#13726=DIRECTION('',(0.,0.,-1.));
#13727=DIRECTION('center_axis',(0.,0.,-1.));
#13728=DIRECTION('ref_axis',(1.,0.,0.));
#13729=DIRECTION('center_axis',(0.,0.,1.));
#13730=DIRECTION('ref_axis',(1.,0.,0.));
#13731=DIRECTION('',(0.,1.,0.));
#13732=DIRECTION('',(0.,-1.,0.));
#13733=DIRECTION('center_axis',(0.,0.,1.));
#13734=DIRECTION('ref_axis',(1.,0.,0.));
#13735=DIRECTION('center_axis',(0.,0.,1.));
#13736=DIRECTION('ref_axis',(1.,0.,0.));
#13737=DIRECTION('',(0.,0.,-1.));
#13738=DIRECTION('center_axis',(0.,0.,-1.));
#13739=DIRECTION('ref_axis',(1.,0.,0.));
#13740=DIRECTION('',(0.,0.,1.));
#13741=DIRECTION('center_axis',(0.,0.,1.));
#13742=DIRECTION('ref_axis',(1.,0.,0.));
#13743=DIRECTION('center_axis',(0.,0.,1.));
#13744=DIRECTION('ref_axis',(1.,0.,0.));
#13745=DIRECTION('',(0.,0.,1.));
#13746=DIRECTION('center_axis',(0.,0.,1.));
#13747=DIRECTION('ref_axis',(1.,0.,0.));
#13748=DIRECTION('',(0.,0.,-1.));
#13749=DIRECTION('center_axis',(0.,0.,-1.));
#13750=DIRECTION('ref_axis',(1.,0.,0.));
#13751=DIRECTION('center_axis',(0.,0.,1.));
#13752=DIRECTION('ref_axis',(1.,0.,0.));
#13753=DIRECTION('',(0.,1.,0.));
#13754=DIRECTION('',(0.,-1.,0.));
#13755=DIRECTION('center_axis',(0.,0.,1.));
#13756=DIRECTION('ref_axis',(1.,0.,0.));
#13757=DIRECTION('center_axis',(1.,0.,0.));
#13758=DIRECTION('ref_axis',(0.,1.,0.));
#13759=DIRECTION('',(0.,1.,0.));
#13760=DIRECTION('',(0.,0.,1.));
#13761=DIRECTION('',(0.,1.,0.));
#13762=DIRECTION('',(0.,0.,1.));
#13763=DIRECTION('',(0.,1.,0.));
#13764=DIRECTION('',(0.,0.,-1.));
#13765=DIRECTION('',(0.,1.,0.));
#13766=DIRECTION('',(0.,0.,1.));
#13767=DIRECTION('',(0.,1.,0.));
#13768=DIRECTION('',(0.,1.,0.));
#13769=DIRECTION('center_axis',(0.,0.,1.));
#13770=DIRECTION('ref_axis',(1.,0.,0.));
#13771=DIRECTION('',(-1.,0.,0.));
#13772=DIRECTION('',(0.,-1.,0.));
#13773=DIRECTION('center_axis',(0.,0.,1.));
#13774=DIRECTION('ref_axis',(1.,0.,0.));
#13775=DIRECTION('',(0.,-1.,0.));
#13776=DIRECTION('',(1.,0.,0.));
#13777=DIRECTION('center_axis',(0.,0.,1.));
#13778=DIRECTION('ref_axis',(1.,0.,0.));
#13779=DIRECTION('',(0.,-1.,0.));
#13780=DIRECTION('center_axis',(0.,0.,1.));
#13781=DIRECTION('ref_axis',(1.,0.,0.));
#13782=DIRECTION('center_axis',(0.,0.,1.));
#13783=DIRECTION('ref_axis',(1.,0.,0.));
#13784=DIRECTION('',(0.,0.,1.));
#13785=DIRECTION('center_axis',(0.,0.,1.));
#13786=DIRECTION('ref_axis',(1.,0.,0.));
#13787=DIRECTION('center_axis',(0.,0.,1.));
#13788=DIRECTION('ref_axis',(1.,0.,0.));
#13789=DIRECTION('',(0.,0.,1.));
#13790=DIRECTION('center_axis',(0.,1.,0.));
#13791=DIRECTION('ref_axis',(-1.,0.,0.));
#13792=DIRECTION('',(-1.,0.,0.));
#13793=DIRECTION('',(0.,0.,1.));
#13794=DIRECTION('',(-1.,0.,0.));
#13795=DIRECTION('center_axis',(0.,-1.,0.));
#13796=DIRECTION('ref_axis',(1.,0.,0.));
#13797=DIRECTION('',(1.,0.,0.));
#13798=DIRECTION('',(0.,0.,-1.));
#13799=DIRECTION('',(1.,0.,0.));
#13800=DIRECTION('center_axis',(0.,0.,1.));
#13801=DIRECTION('ref_axis',(1.,0.,0.));
#13802=DIRECTION('',(0.,-1.,0.));
#13803=DIRECTION('center_axis',(-1.,0.,0.));
#13804=DIRECTION('ref_axis',(0.,-1.,0.));
#13805=DIRECTION('',(0.,0.,1.));
#13806=DIRECTION('',(0.,-1.,0.));
#13807=DIRECTION('',(0.,-1.,0.));
#13808=DIRECTION('',(0.,0.,1.));
#13809=DIRECTION('center_axis',(0.,0.,1.));
#13810=DIRECTION('ref_axis',(1.,0.,0.));
#13811=DIRECTION('',(1.,0.,0.));
#13812=DIRECTION('center_axis',(0.,0.,1.));
#13813=DIRECTION('ref_axis',(1.,0.,0.));
#13814=DIRECTION('',(-1.,0.,0.));
#13815=DIRECTION('center_axis',(0.,1.,0.));
#13816=DIRECTION('ref_axis',(-1.,0.,0.));
#13817=DIRECTION('center_axis',(0.,-1.,0.));
#13818=DIRECTION('ref_axis',(1.,0.,0.));
#13819=DIRECTION('axis',(0.,0.,1.));
#13820=DIRECTION('refdir',(1.,0.,0.));
#13821=DIRECTION('center_axis',(0.,0.,1.));
#13822=DIRECTION('ref_axis',(1.,0.,0.));
#13823=DIRECTION('',(0.,0.,-1.));
#13824=DIRECTION('center_axis',(0.,0.,-1.));
#13825=DIRECTION('ref_axis',(1.,0.,0.));
#13826=DIRECTION('',(0.,0.,1.));
#13827=DIRECTION('center_axis',(0.,0.,1.));
#13828=DIRECTION('ref_axis',(1.,0.,0.));
#13829=DIRECTION('center_axis',(0.,0.,1.));
#13830=DIRECTION('ref_axis',(1.,0.,0.));
#13831=DIRECTION('',(0.,0.,1.));
#13832=DIRECTION('center_axis',(0.,0.,1.));
#13833=DIRECTION('ref_axis',(1.,0.,0.));
#13834=DIRECTION('',(0.,0.,-1.));
#13835=DIRECTION('center_axis',(0.,0.,-1.));
#13836=DIRECTION('ref_axis',(1.,0.,0.));
#13837=DIRECTION('center_axis',(0.,0.,1.));
#13838=DIRECTION('ref_axis',(1.,0.,0.));
#13839=DIRECTION('',(0.,1.,0.));
#13840=DIRECTION('',(0.,-1.,0.));
#13841=DIRECTION('center_axis',(0.,0.,1.));
#13842=DIRECTION('ref_axis',(1.,0.,0.));
#13843=DIRECTION('center_axis',(0.,0.,1.));
#13844=DIRECTION('ref_axis',(1.,0.,0.));
#13845=DIRECTION('',(0.,0.,-1.));
#13846=DIRECTION('center_axis',(0.,0.,-1.));
#13847=DIRECTION('ref_axis',(1.,0.,0.));
#13848=DIRECTION('',(0.,0.,1.));
#13849=DIRECTION('center_axis',(0.,0.,1.));
#13850=DIRECTION('ref_axis',(1.,0.,0.));
#13851=DIRECTION('center_axis',(0.,0.,1.));
#13852=DIRECTION('ref_axis',(1.,0.,0.));
#13853=DIRECTION('',(0.,0.,1.));
#13854=DIRECTION('center_axis',(0.,0.,1.));
#13855=DIRECTION('ref_axis',(1.,0.,0.));
#13856=DIRECTION('',(0.,0.,-1.));
#13857=DIRECTION('center_axis',(0.,0.,-1.));
#13858=DIRECTION('ref_axis',(1.,0.,0.));
#13859=DIRECTION('center_axis',(0.,0.,1.));
#13860=DIRECTION('ref_axis',(1.,0.,0.));
#13861=DIRECTION('',(0.,1.,0.));
#13862=DIRECTION('',(0.,-1.,0.));
#13863=DIRECTION('center_axis',(0.,0.,1.));
#13864=DIRECTION('ref_axis',(1.,0.,0.));
#13865=DIRECTION('center_axis',(1.,0.,0.));
#13866=DIRECTION('ref_axis',(0.,1.,0.));
#13867=DIRECTION('',(0.,1.,0.));
#13868=DIRECTION('',(0.,0.,1.));
#13869=DIRECTION('',(0.,1.,0.));
#13870=DIRECTION('',(0.,0.,1.));
#13871=DIRECTION('',(0.,1.,0.));
#13872=DIRECTION('',(0.,0.,-1.));
#13873=DIRECTION('',(0.,1.,0.));
#13874=DIRECTION('',(0.,0.,1.));
#13875=DIRECTION('',(0.,1.,0.));
#13876=DIRECTION('',(0.,1.,0.));
#13877=DIRECTION('center_axis',(0.,0.,1.));
#13878=DIRECTION('ref_axis',(1.,0.,0.));
#13879=DIRECTION('',(-1.,0.,0.));
#13880=DIRECTION('',(0.,-1.,0.));
#13881=DIRECTION('center_axis',(0.,0.,1.));
#13882=DIRECTION('ref_axis',(1.,0.,0.));
#13883=DIRECTION('',(0.,-1.,0.));
#13884=DIRECTION('',(1.,0.,0.));
#13885=DIRECTION('center_axis',(0.,0.,1.));
#13886=DIRECTION('ref_axis',(1.,0.,0.));
#13887=DIRECTION('',(0.,-1.,0.));
#13888=DIRECTION('center_axis',(0.,0.,1.));
#13889=DIRECTION('ref_axis',(1.,0.,0.));
#13890=DIRECTION('center_axis',(0.,0.,1.));
#13891=DIRECTION('ref_axis',(1.,0.,0.));
#13892=DIRECTION('',(0.,0.,1.));
#13893=DIRECTION('center_axis',(0.,0.,1.));
#13894=DIRECTION('ref_axis',(1.,0.,0.));
#13895=DIRECTION('center_axis',(0.,0.,1.));
#13896=DIRECTION('ref_axis',(1.,0.,0.));
#13897=DIRECTION('',(0.,0.,1.));
#13898=DIRECTION('center_axis',(0.,1.,0.));
#13899=DIRECTION('ref_axis',(-1.,0.,0.));
#13900=DIRECTION('',(-1.,0.,0.));
#13901=DIRECTION('',(0.,0.,1.));
#13902=DIRECTION('',(-1.,0.,0.));
#13903=DIRECTION('center_axis',(0.,-1.,0.));
#13904=DIRECTION('ref_axis',(1.,0.,0.));
#13905=DIRECTION('',(1.,0.,0.));
#13906=DIRECTION('',(0.,0.,-1.));
#13907=DIRECTION('',(1.,0.,0.));
#13908=DIRECTION('center_axis',(0.,0.,1.));
#13909=DIRECTION('ref_axis',(1.,0.,0.));
#13910=DIRECTION('',(0.,-1.,0.));
#13911=DIRECTION('center_axis',(-1.,0.,0.));
#13912=DIRECTION('ref_axis',(0.,-1.,0.));
#13913=DIRECTION('',(0.,0.,1.));
#13914=DIRECTION('',(0.,-1.,0.));
#13915=DIRECTION('',(0.,-1.,0.));
#13916=DIRECTION('',(0.,0.,1.));
#13917=DIRECTION('center_axis',(0.,0.,1.));
#13918=DIRECTION('ref_axis',(1.,0.,0.));
#13919=DIRECTION('',(1.,0.,0.));
#13920=DIRECTION('center_axis',(0.,0.,1.));
#13921=DIRECTION('ref_axis',(1.,0.,0.));
#13922=DIRECTION('',(-1.,0.,0.));
#13923=DIRECTION('center_axis',(0.,1.,0.));
#13924=DIRECTION('ref_axis',(-1.,0.,0.));
#13925=DIRECTION('center_axis',(0.,-1.,0.));
#13926=DIRECTION('ref_axis',(1.,0.,0.));
#13927=DIRECTION('axis',(0.,0.,1.));
#13928=DIRECTION('refdir',(1.,0.,0.));
#13929=DIRECTION('axis',(0.,0.,1.));
#13930=DIRECTION('refdir',(1.,0.,0.));
#13931=DIRECTION('center_axis',(0.,-1.,0.));
#13932=DIRECTION('ref_axis',(0.,0.,-1.));
#13933=DIRECTION('center_axis',(0.,-1.,0.));
#13934=DIRECTION('ref_axis',(1.,0.,0.));
#13935=DIRECTION('center_axis',(0.,-1.,0.));
#13936=DIRECTION('ref_axis',(1.,0.,0.));
#13937=DIRECTION('center_axis',(1.,0.,1.22464679914735E-16));
#13938=DIRECTION('ref_axis',(-1.22464679914735E-16,0.,1.));
#13939=DIRECTION('center_axis',(0.,1.,0.));
#13940=DIRECTION('ref_axis',(1.,0.,0.));
#13941=DIRECTION('center_axis',(0.,1.,0.));
#13942=DIRECTION('ref_axis',(1.,0.,0.));
#13943=DIRECTION('center_axis',(0.,-1.,0.));
#13944=DIRECTION('ref_axis',(1.,0.,0.));
#13945=DIRECTION('',(0.,1.,0.));
#13946=DIRECTION('center_axis',(0.,-1.,0.));
#13947=DIRECTION('ref_axis',(1.,0.,0.));
#13948=DIRECTION('center_axis',(0.,-1.,0.));
#13949=DIRECTION('ref_axis',(1.,0.,0.));
#13950=DIRECTION('center_axis',(0.,-1.,0.));
#13951=DIRECTION('ref_axis',(1.,0.,0.));
#13952=DIRECTION('',(0.,1.,0.));
#13953=DIRECTION('center_axis',(0.,-1.,0.));
#13954=DIRECTION('ref_axis',(1.,0.,0.));
#13955=DIRECTION('center_axis',(0.,1.,0.));
#13956=DIRECTION('ref_axis',(1.,0.,0.));
#13957=DIRECTION('',(-0.707106781186547,0.707106781186548,-8.65956056235493E-17));
#13958=DIRECTION('center_axis',(0.,-1.,0.));
#13959=DIRECTION('ref_axis',(1.,0.,0.));
#13960=DIRECTION('center_axis',(0.,1.,0.));
#13961=DIRECTION('ref_axis',(0.,0.,1.));
#13962=DIRECTION('center_axis',(0.,-1.,0.));
#13963=DIRECTION('ref_axis',(1.,0.,0.));
#13964=DIRECTION('center_axis',(0.,-1.,0.));
#13965=DIRECTION('ref_axis',(1.,0.,0.));
#13966=DIRECTION('',(0.,1.,0.));
#13967=DIRECTION('center_axis',(0.,-1.,0.));
#13968=DIRECTION('ref_axis',(0.,0.,-1.));
#13969=DIRECTION('center_axis',(0.,-1.,0.));
#13970=DIRECTION('ref_axis',(1.,0.,0.));
#13971=DIRECTION('center_axis',(0.,-1.,0.));
#13972=DIRECTION('ref_axis',(1.,0.,0.));
#13973=DIRECTION('',(0.707106781186547,0.707106781186548,8.65956056235493E-17));
#13974=DIRECTION('axis',(0.,0.,1.));
#13975=DIRECTION('refdir',(1.,0.,0.));
#13976=DIRECTION('center_axis',(0.,-1.,0.));
#13977=DIRECTION('ref_axis',(0.,0.,-1.));
#13978=DIRECTION('center_axis',(0.,-1.,0.));
#13979=DIRECTION('ref_axis',(1.,0.,0.));
#13980=DIRECTION('center_axis',(0.,-1.,0.));
#13981=DIRECTION('ref_axis',(1.,0.,0.));
#13982=DIRECTION('center_axis',(1.,0.,1.22464679914735E-16));
#13983=DIRECTION('ref_axis',(-1.22464679914735E-16,0.,1.));
#13984=DIRECTION('center_axis',(0.,1.,0.));
#13985=DIRECTION('ref_axis',(1.,0.,0.));
#13986=DIRECTION('center_axis',(0.,1.,0.));
#13987=DIRECTION('ref_axis',(1.,0.,0.));
#13988=DIRECTION('center_axis',(0.,-1.,0.));
#13989=DIRECTION('ref_axis',(1.,0.,0.));
#13990=DIRECTION('center_axis',(0.,-1.,0.));
#13991=DIRECTION('ref_axis',(1.,0.,0.));
#13992=DIRECTION('',(0.,1.,0.));
#13993=DIRECTION('center_axis',(0.,1.,0.));
#13994=DIRECTION('ref_axis',(0.,0.,1.));
#13995=DIRECTION('center_axis',(0.,-1.,0.));
#13996=DIRECTION('ref_axis',(1.,0.,0.));
#13997=DIRECTION('center_axis',(0.,-1.,0.));
#13998=DIRECTION('ref_axis',(1.,0.,0.));
#13999=DIRECTION('center_axis',(0.,-1.,0.));
#14000=DIRECTION('ref_axis',(1.,0.,0.));
#14001=DIRECTION('center_axis',(0.,-1.,0.));
#14002=DIRECTION('ref_axis',(1.,0.,0.));
#14003=DIRECTION('',(0.707106781186548,0.707106781186547,8.65956056235494E-17));
#14004=DIRECTION('center_axis',(0.,-1.,0.));
#14005=DIRECTION('ref_axis',(1.,0.,0.));
#14006=DIRECTION('center_axis',(0.,-1.,0.));
#14007=DIRECTION('ref_axis',(1.,0.,0.));
#14008=DIRECTION('',(0.,1.,0.));
#14009=DIRECTION('center_axis',(0.,1.,0.));
#14010=DIRECTION('ref_axis',(1.,0.,0.));
#14011=DIRECTION('center_axis',(0.,-1.,0.));
#14012=DIRECTION('ref_axis',(1.,0.,0.));
#14013=DIRECTION('',(-0.707106781186548,0.707106781186547,-8.65956056235494E-17));
#14014=DIRECTION('center_axis',(0.,-1.,0.));
#14015=DIRECTION('ref_axis',(0.,0.,-1.));
#14016=DIRECTION('center_axis',(0.,-1.,0.));
#14017=DIRECTION('ref_axis',(1.,0.,0.));
#14018=DIRECTION('',(0.,1.,0.));
#14019=DIRECTION('axis',(0.,0.,1.));
#14020=DIRECTION('refdir',(1.,0.,0.));
#14021=DIRECTION('center_axis',(0.,0.,1.));
#14022=DIRECTION('ref_axis',(1.,0.,0.));
#14023=DIRECTION('center_axis',(1.22464679914735E-16,-1.,0.));
#14024=DIRECTION('ref_axis',(-1.,-1.22464679914735E-16,0.));
#14025=DIRECTION('center_axis',(0.707106781186548,0.,0.707106781186548));
#14026=DIRECTION('ref_axis',(0.707106781186548,0.,-0.707106781186548));
#14027=DIRECTION('center_axis',(8.65956056235494E-17,-1.,-8.65956056235493E-17));
#14028=DIRECTION('ref_axis',(-0.707106781186547,-1.22464679914735E-16,0.707106781186547));
#14029=DIRECTION('center_axis',(1.,0.,0.));
#14030=DIRECTION('ref_axis',(6.12323399573676E-17,0.,-1.));
#14031=DIRECTION('center_axis',(7.49879891330929E-33,-1.,-1.22464679914735E-16));
#14032=DIRECTION('ref_axis',(-6.12323399573676E-17,-1.22464679914735E-16,
1.));
#14033=DIRECTION('center_axis',(0.707106781186548,0.,-0.707106781186548));
#14034=DIRECTION('ref_axis',(-0.707106781186548,0.,-0.707106781186548));
#14035=DIRECTION('center_axis',(-8.65956056235493E-17,-1.,-8.65956056235494E-17));
#14036=DIRECTION('ref_axis',(0.707106781186547,-1.22464679914735E-16,0.707106781186547));
#14037=DIRECTION('center_axis',(0.,0.,-1.));
#14038=DIRECTION('ref_axis',(-1.,0.,-1.22464679914735E-16));
#14039=DIRECTION('center_axis',(-1.22464679914735E-16,-1.,-1.49975978266186E-32));
#14040=DIRECTION('ref_axis',(1.,-1.22464679914735E-16,1.22464679914735E-16));
#14041=DIRECTION('center_axis',(-0.707106781186547,0.,-0.707106781186548));
#14042=DIRECTION('ref_axis',(-0.707106781186548,0.,0.707106781186547));
#14043=DIRECTION('center_axis',(-8.65956056235493E-17,-1.,8.65956056235493E-17));
#14044=DIRECTION('ref_axis',(0.707106781186548,-1.22464679914735E-16,-0.707106781186547));
#14045=DIRECTION('center_axis',(-1.,0.,0.));
#14046=DIRECTION('ref_axis',(-1.83697019872103E-16,0.,1.));
#14047=DIRECTION('center_axis',(-2.24963967399279E-32,-1.,1.22464679914735E-16));
#14048=DIRECTION('ref_axis',(1.83697019872103E-16,-1.22464679914735E-16,
-1.));
#14049=DIRECTION('center_axis',(-0.707106781186548,0.,0.707106781186548));
#14050=DIRECTION('ref_axis',(0.707106781186547,0.,0.707106781186548));
#14051=DIRECTION('center_axis',(8.65956056235493E-17,-1.,8.65956056235493E-17));
#14052=DIRECTION('ref_axis',(-0.707106781186547,-1.22464679914735E-16,-0.707106781186548));
#14053=DIRECTION('axis',(0.,0.,1.));
#14054=DIRECTION('refdir',(1.,0.,0.));
#14055=DIRECTION('center_axis',(0.,0.,1.));
#14056=DIRECTION('ref_axis',(1.,0.,0.));
#14057=DIRECTION('center_axis',(0.,-1.,0.));
#14058=DIRECTION('ref_axis',(0.,0.,-1.));
#14059=DIRECTION('center_axis',(0.,-1.,0.));
#14060=DIRECTION('ref_axis',(0.,0.,-1.));
#14061=DIRECTION('center_axis',(0.,1.,0.));
#14062=DIRECTION('ref_axis',(1.,0.,0.));
#14063=DIRECTION('center_axis',(0.,1.,0.));
#14064=DIRECTION('ref_axis',(1.,0.,0.));
#14065=DIRECTION('center_axis',(0.,1.,0.));
#14066=DIRECTION('ref_axis',(1.,0.,0.));
#14067=DIRECTION('center_axis',(0.,1.,0.));
#14068=DIRECTION('ref_axis',(1.,0.,0.));
#14069=DIRECTION('',(0.,-1.,0.));
#14070=DIRECTION('center_axis',(0.,-1.,0.));
#14071=DIRECTION('ref_axis',(1.,0.,0.));
#14072=DIRECTION('center_axis',(0.,1.,0.));
#14073=DIRECTION('ref_axis',(1.,0.,0.));
#14074=DIRECTION('center_axis',(0.,1.,0.));
#14075=DIRECTION('ref_axis',(1.,0.,0.));
#14076=DIRECTION('center_axis',(0.,1.,0.));
#14077=DIRECTION('ref_axis',(1.,0.,0.));
#14078=DIRECTION('center_axis',(0.,1.,0.));
#14079=DIRECTION('ref_axis',(1.,0.,0.));
#14080=DIRECTION('center_axis',(0.,1.,0.));
#14081=DIRECTION('ref_axis',(1.,0.,0.));
#14082=DIRECTION('center_axis',(0.,1.,0.));
#14083=DIRECTION('ref_axis',(1.,0.,0.));
#14084=DIRECTION('center_axis',(0.,-1.,0.));
#14085=DIRECTION('ref_axis',(1.,0.,0.));
#14086=DIRECTION('center_axis',(0.,-1.,0.));
#14087=DIRECTION('ref_axis',(0.,0.,-1.));
#14088=DIRECTION('center_axis',(6.12323399573677E-17,0.,1.));
#14089=DIRECTION('ref_axis',(1.,0.,0.));
#14090=DIRECTION('center_axis',(0.,-1.,0.));
#14091=DIRECTION('ref_axis',(0.,0.,-1.));
#14092=DIRECTION('center_axis',(0.,1.,0.));
#14093=DIRECTION('ref_axis',(1.,0.,0.));
#14094=DIRECTION('center_axis',(0.,-1.,0.));
#14095=DIRECTION('ref_axis',(1.,0.,0.));
#14096=DIRECTION('center_axis',(0.,-1.,0.));
#14097=DIRECTION('ref_axis',(0.,0.,-1.));
#14098=DIRECTION('center_axis',(0.,0.,1.));
#14099=DIRECTION('ref_axis',(1.,0.,0.));
#14100=DIRECTION('center_axis',(0.,-1.,0.));
#14101=DIRECTION('ref_axis',(0.,0.,-1.));
#14102=DIRECTION('center_axis',(0.,1.,0.));
#14103=DIRECTION('ref_axis',(1.,0.,0.));
#14104=DIRECTION('center_axis',(0.,-1.,0.));
#14105=DIRECTION('ref_axis',(1.,0.,0.));
#14106=DIRECTION('center_axis',(0.,-1.,0.));
#14107=DIRECTION('ref_axis',(0.,0.,-1.));
#14108=DIRECTION('center_axis',(0.,0.,1.));
#14109=DIRECTION('ref_axis',(1.,0.,0.));
#14110=DIRECTION('center_axis',(0.,-1.,0.));
#14111=DIRECTION('ref_axis',(0.,0.,-1.));
#14112=DIRECTION('center_axis',(0.,1.,0.));
#14113=DIRECTION('ref_axis',(1.,0.,0.));
#14114=DIRECTION('center_axis',(0.,-1.,0.));
#14115=DIRECTION('ref_axis',(1.,0.,0.));
#14116=DIRECTION('center_axis',(0.,-1.,0.));
#14117=DIRECTION('ref_axis',(0.,0.,-1.));
#14118=DIRECTION('center_axis',(0.,0.,1.));
#14119=DIRECTION('ref_axis',(1.,0.,0.));
#14120=DIRECTION('center_axis',(0.,-1.,0.));
#14121=DIRECTION('ref_axis',(0.,0.,-1.));
#14122=DIRECTION('center_axis',(0.,1.,0.));
#14123=DIRECTION('ref_axis',(1.,0.,0.));
#14124=DIRECTION('center_axis',(0.,-1.,0.));
#14125=DIRECTION('ref_axis',(1.,0.,0.));
#14126=DIRECTION('center_axis',(0.,-1.,0.));
#14127=DIRECTION('ref_axis',(0.,0.,-1.));
#14128=DIRECTION('center_axis',(6.12323399573676E-17,0.,1.));
#14129=DIRECTION('ref_axis',(1.,0.,0.));
#14130=DIRECTION('center_axis',(0.,-1.,0.));
#14131=DIRECTION('ref_axis',(0.,0.,-1.));
#14132=DIRECTION('center_axis',(0.,1.,0.));
#14133=DIRECTION('ref_axis',(1.,0.,0.));
#14134=DIRECTION('center_axis',(0.,-1.,0.));
#14135=DIRECTION('ref_axis',(1.,0.,0.));
#14136=DIRECTION('center_axis',(0.,-1.,0.));
#14137=DIRECTION('ref_axis',(0.,0.,-1.));
#14138=DIRECTION('center_axis',(0.,0.,1.));
#14139=DIRECTION('ref_axis',(1.,0.,0.));
#14140=DIRECTION('center_axis',(0.,-1.,0.));
#14141=DIRECTION('ref_axis',(0.,0.,-1.));
#14142=DIRECTION('center_axis',(0.,1.,0.));
#14143=DIRECTION('ref_axis',(1.,0.,0.));
#14144=DIRECTION('center_axis',(0.,1.,0.));
#14145=DIRECTION('ref_axis',(1.,0.,0.));
#14146=DIRECTION('',(0.,1.,0.));
#14147=DIRECTION('center_axis',(0.,-1.,0.));
#14148=DIRECTION('ref_axis',(1.,0.,0.));
#14149=DIRECTION('center_axis',(0.,-1.,0.));
#14150=DIRECTION('ref_axis',(1.,0.,0.));
#14151=DIRECTION('center_axis',(0.,1.,0.));
#14152=DIRECTION('ref_axis',(1.,0.,0.));
#14153=DIRECTION('center_axis',(0.,-1.,0.));
#14154=DIRECTION('ref_axis',(0.,0.,-1.));
#14155=DIRECTION('center_axis',(0.,0.,1.));
#14156=DIRECTION('ref_axis',(1.,0.,0.));
#14157=DIRECTION('center_axis',(0.,-1.,0.));
#14158=DIRECTION('ref_axis',(0.,0.,-1.));
#14159=DIRECTION('center_axis',(0.,-1.,0.));
#14160=DIRECTION('ref_axis',(-1.,0.,0.));
#14161=DIRECTION('center_axis',(0.,1.,0.));
#14162=DIRECTION('ref_axis',(1.,0.,0.));
#14163=DIRECTION('axis',(0.,0.,1.));
#14164=DIRECTION('refdir',(1.,0.,0.));
#14165=DIRECTION('center_axis',(0.,1.,0.));
#14166=DIRECTION('ref_axis',(0.,0.,1.));
#14167=DIRECTION('center_axis',(0.,-1.,0.));
#14168=DIRECTION('ref_axis',(1.,0.,0.));
#14169=DIRECTION('center_axis',(0.,-1.,0.));
#14170=DIRECTION('ref_axis',(1.,0.,0.));
#14171=DIRECTION('center_axis',(0.,-1.,0.));
#14172=DIRECTION('ref_axis',(1.,0.,0.));
#14173=DIRECTION('center_axis',(0.,-1.,0.));
#14174=DIRECTION('ref_axis',(1.,0.,0.));
#14175=DIRECTION('',(0.,1.,0.));
#14176=DIRECTION('center_axis',(0.,-1.,0.));
#14177=DIRECTION('ref_axis',(0.,0.,-1.));
#14178=DIRECTION('center_axis',(0.,-1.,0.));
#14179=DIRECTION('ref_axis',(1.,0.,0.));
#14180=DIRECTION('center_axis',(0.,-1.,0.));
#14181=DIRECTION('ref_axis',(1.,0.,0.));
#14182=DIRECTION('',(0.,1.,0.));
#14183=DIRECTION('center_axis',(0.,1.,0.));
#14184=DIRECTION('ref_axis',(0.,0.,1.));
#14185=DIRECTION('center_axis',(0.,-1.,0.));
#14186=DIRECTION('ref_axis',(1.,0.,0.));
#14187=DIRECTION('center_axis',(0.,-1.,0.));
#14188=DIRECTION('ref_axis',(1.,0.,0.));
#14189=DIRECTION('center_axis',(0.,-1.,0.));
#14190=DIRECTION('ref_axis',(1.,0.,0.));
#14191=DIRECTION('center_axis',(0.,-1.,0.));
#14192=DIRECTION('ref_axis',(1.,0.,0.));
#14193=DIRECTION('',(0.,1.,0.));
#14194=DIRECTION('center_axis',(0.,-1.,0.));
#14195=DIRECTION('ref_axis',(0.,0.,-1.));
#14196=DIRECTION('center_axis',(0.,-1.,0.));
#14197=DIRECTION('ref_axis',(1.,0.,0.));
#14198=DIRECTION('center_axis',(0.,-1.,0.));
#14199=DIRECTION('ref_axis',(1.,0.,0.));
#14200=DIRECTION('',(0.,1.,0.));
#14201=DIRECTION('',(0.,0.,1.));
#14202=DIRECTION('',(1.,0.,0.));
#14203=DIRECTION('',(0.,0.,1.));
#14204=DIRECTION('',(1.,0.,0.));
#14205=DIRECTION('',(0.,0.,1.));
#14206=DIRECTION('',(1.,0.,0.));
#14207=DIRECTION('',(0.,0.,1.));
#14208=DIRECTION('',(1.,0.,0.));
#14209=DIRECTION('',(0.,0.,1.));
#14210=DIRECTION('',(1.,0.,0.));
#14211=DIRECTION('axis',(0.,0.,1.));
#14212=DIRECTION('refdir',(1.,0.,0.));
#14213=DIRECTION('center_axis',(0.,0.,-1.));
#14214=DIRECTION('ref_axis',(0.,1.,0.));
#14215=DIRECTION('',(0.,1.,0.));
#14216=DIRECTION('',(1.,0.,0.));
#14217=DIRECTION('',(0.,-1.,0.));
#14218=DIRECTION('',(1.,0.,0.));
#14219=DIRECTION('center_axis',(0.,1.,-8.88178419700125E-16));
#14220=DIRECTION('ref_axis',(0.,8.88178419700125E-16,1.));
#14221=DIRECTION('',(0.,8.88178419700125E-16,1.));
#14222=DIRECTION('',(1.,0.,0.));
#14223=DIRECTION('',(0.,-8.88178419700125E-16,-1.));
#14224=DIRECTION('center_axis',(0.,-7.40148683083439E-16,-1.));
#14225=DIRECTION('ref_axis',(0.,1.,-7.40148683083439E-16));
#14226=DIRECTION('',(0.,1.,-7.40148683083439E-16));
#14227=DIRECTION('',(1.,0.,0.));
#14228=DIRECTION('',(0.,-1.,7.40148683083439E-16));
#14229=DIRECTION('center_axis',(0.,-0.707106781186547,-0.707106781186548));
#14230=DIRECTION('ref_axis',(0.,0.707106781186548,-0.707106781186547));
#14231=DIRECTION('',(0.,0.707106781186548,-0.707106781186547));
#14232=DIRECTION('',(1.,0.,0.));
#14233=DIRECTION('',(0.,-0.707106781186548,0.707106781186547));
#14234=DIRECTION('center_axis',(0.,-1.,2.77555756156289E-16));
#14235=DIRECTION('ref_axis',(0.,-2.77555756156289E-16,-1.));
#14236=DIRECTION('',(0.,-2.77555756156289E-16,-1.));
#14237=DIRECTION('',(1.,0.,0.));
#14238=DIRECTION('',(0.,2.77555756156289E-16,1.));
#14239=DIRECTION('center_axis',(0.,-0.707106781186547,0.707106781186548));
#14240=DIRECTION('ref_axis',(0.,-0.707106781186548,-0.707106781186547));
#14241=DIRECTION('',(0.,-0.707106781186548,-0.707106781186547));
#14242=DIRECTION('',(1.,0.,0.));
#14243=DIRECTION('',(0.,0.707106781186548,0.707106781186547));
#14244=DIRECTION('center_axis',(0.,7.40148683083438E-16,1.));
#14245=DIRECTION('ref_axis',(0.,-1.,7.40148683083438E-16));
#14246=DIRECTION('',(0.,-1.,7.40148683083438E-16));
#14247=DIRECTION('',(1.,0.,0.));
#14248=DIRECTION('',(0.,1.,-7.40148683083438E-16));
#14249=DIRECTION('center_axis',(0.,1.,-4.44089209850063E-16));
#14250=DIRECTION('ref_axis',(0.,4.44089209850063E-16,1.));
#14251=DIRECTION('',(0.,4.44089209850063E-16,1.));
#14252=DIRECTION('',(1.,0.,0.));
#14253=DIRECTION('',(0.,-4.44089209850063E-16,-1.));
#14254=DIRECTION('center_axis',(0.,2.41352831440251E-16,1.));
#14255=DIRECTION('ref_axis',(0.,-1.,2.41352831440251E-16));
#14256=DIRECTION('',(0.,-1.,2.41352831440251E-16));
#14257=DIRECTION('',(-1.,0.,0.));
#14258=DIRECTION('',(0.,1.,-2.41352831440251E-16));
#14259=DIRECTION('center_axis',(0.,-1.,2.41352831440251E-16));
#14260=DIRECTION('ref_axis',(0.,-2.41352831440251E-16,-1.));
#14261=DIRECTION('',(0.,-2.41352831440251E-16,-1.));
#14262=DIRECTION('',(1.,0.,0.));
#14263=DIRECTION('',(0.,2.41352831440251E-16,1.));
#14264=DIRECTION('',(1.,0.,0.));
#14265=DIRECTION('center_axis',(0.,0.,-1.));
#14266=DIRECTION('ref_axis',(0.,1.,0.));
#14267=DIRECTION('',(0.,1.,0.));
#14268=DIRECTION('',(1.,0.,0.));
#14269=DIRECTION('',(0.,-1.,0.));
#14270=DIRECTION('center_axis',(0.,-1.,0.));
#14271=DIRECTION('ref_axis',(0.,0.,-1.));
#14272=DIRECTION('',(0.,0.,-1.));
#14273=DIRECTION('',(1.,0.,0.));
#14274=DIRECTION('',(0.,0.,1.));
#14275=DIRECTION('center_axis',(0.,-0.707106781186547,0.707106781186548));
#14276=DIRECTION('ref_axis',(0.,-0.707106781186548,-0.707106781186547));
#14277=DIRECTION('',(0.,-0.707106781186548,-0.707106781186547));
#14278=DIRECTION('',(1.,0.,0.));
#14279=DIRECTION('',(0.,0.707106781186548,0.707106781186547));
#14280=DIRECTION('center_axis',(0.,0.,1.));
#14281=DIRECTION('ref_axis',(0.,-1.,0.));
#14282=DIRECTION('',(0.,-1.,0.));
#14283=DIRECTION('',(1.,0.,0.));
#14284=DIRECTION('',(0.,1.,0.));
#14285=DIRECTION('center_axis',(0.,0.707106781186548,0.707106781186547));
#14286=DIRECTION('ref_axis',(0.,-0.707106781186547,0.707106781186548));
#14287=DIRECTION('',(0.,-0.707106781186547,0.707106781186548));
#14288=DIRECTION('',(1.,0.,0.));
#14289=DIRECTION('',(0.,0.707106781186547,-0.707106781186548));
#14290=DIRECTION('center_axis',(0.,1.,0.));
#14291=DIRECTION('ref_axis',(0.,0.,1.));
#14292=DIRECTION('',(0.,0.,1.));
#14293=DIRECTION('',(1.,0.,0.));
#14294=DIRECTION('',(0.,0.,-1.));
#14295=DIRECTION('center_axis',(0.,0.,-1.));
#14296=DIRECTION('ref_axis',(0.,1.,0.));
#14297=DIRECTION('',(0.,1.,0.));
#14298=DIRECTION('',(1.,0.,0.));
#14299=DIRECTION('',(0.,-1.,0.));
#14300=DIRECTION('center_axis',(0.,1.,-2.41352831440251E-16));
#14301=DIRECTION('ref_axis',(0.,2.41352831440251E-16,1.));
#14302=DIRECTION('',(0.,2.41352831440251E-16,1.));
#14303=DIRECTION('',(-1.,0.,0.));
#14304=DIRECTION('',(0.,-2.41352831440251E-16,-1.));
#14305=DIRECTION('center_axis',(0.,0.,1.));
#14306=DIRECTION('ref_axis',(0.,-1.,0.));
#14307=DIRECTION('',(0.,-1.,0.));
#14308=DIRECTION('',(1.,0.,0.));
#14309=DIRECTION('',(0.,1.,0.));
#14310=DIRECTION('',(1.,0.,0.));
#14311=DIRECTION('center_axis',(0.,-1.,0.));
#14312=DIRECTION('ref_axis',(0.,0.,-1.));
#14313=DIRECTION('',(0.,0.,-1.));
#14314=DIRECTION('',(1.,0.,0.));
#14315=DIRECTION('',(0.,0.,1.));
#14316=DIRECTION('center_axis',(0.,0.,1.));
#14317=DIRECTION('ref_axis',(0.,-1.,0.));
#14318=DIRECTION('',(0.,-1.,0.));
#14319=DIRECTION('',(1.,0.,0.));
#14320=DIRECTION('',(0.,1.,0.));
#14321=DIRECTION('center_axis',(0.,0.707106781186548,0.707106781186548));
#14322=DIRECTION('ref_axis',(0.,-0.707106781186548,0.707106781186548));
#14323=DIRECTION('',(0.,-0.707106781186548,0.707106781186548));
#14324=DIRECTION('',(1.,0.,0.));
#14325=DIRECTION('',(0.,0.707106781186548,-0.707106781186548));
#14326=DIRECTION('center_axis',(0.,1.,0.));
#14327=DIRECTION('ref_axis',(0.,0.,1.));
#14328=DIRECTION('',(0.,0.,1.));
#14329=DIRECTION('',(1.,0.,0.));
#14330=DIRECTION('',(0.,0.,-1.));
#14331=DIRECTION('center_axis',(0.,0.707106781186548,-0.707106781186547));
#14332=DIRECTION('ref_axis',(0.,0.707106781186547,0.707106781186548));
#14333=DIRECTION('',(0.,0.707106781186547,0.707106781186548));
#14334=DIRECTION('',(1.,0.,0.));
#14335=DIRECTION('',(0.,-0.707106781186547,-0.707106781186548));
#14336=DIRECTION('center_axis',(0.,-7.40148683083438E-16,-1.));
#14337=DIRECTION('ref_axis',(0.,1.,-7.40148683083438E-16));
#14338=DIRECTION('',(0.,1.,-7.40148683083438E-16));
#14339=DIRECTION('',(1.,0.,0.));
#14340=DIRECTION('',(0.,-1.,7.40148683083438E-16));
#14341=DIRECTION('center_axis',(0.,-1.,0.));
#14342=DIRECTION('ref_axis',(0.,0.,-1.));
#14343=DIRECTION('',(0.,0.,-1.));
#14344=DIRECTION('',(1.,0.,0.));
#14345=DIRECTION('',(0.,0.,1.));
#14346=DIRECTION('center_axis',(0.,0.,-1.));
#14347=DIRECTION('ref_axis',(0.,1.,0.));
#14348=DIRECTION('',(0.,1.,0.));
#14349=DIRECTION('',(-1.,0.,0.));
#14350=DIRECTION('',(0.,-1.,0.));
#14351=DIRECTION('center_axis',(0.,1.,0.));
#14352=DIRECTION('ref_axis',(0.,0.,1.));
#14353=DIRECTION('',(0.,0.,1.));
#14354=DIRECTION('',(1.,0.,0.));
#14355=DIRECTION('',(0.,0.,-1.));
#14356=DIRECTION('',(1.,0.,0.));
#14357=DIRECTION('center_axis',(0.,0.,1.));
#14358=DIRECTION('ref_axis',(0.,-1.,0.));
#14359=DIRECTION('',(0.,-1.,0.));
#14360=DIRECTION('',(1.,0.,0.));
#14361=DIRECTION('',(0.,1.,0.));
#14362=DIRECTION('center_axis',(0.,1.,0.));
#14363=DIRECTION('ref_axis',(0.,0.,1.));
#14364=DIRECTION('',(0.,0.,1.));
#14365=DIRECTION('',(1.,0.,0.));
#14366=DIRECTION('',(0.,0.,-1.));
#14367=DIRECTION('center_axis',(0.,0.707106781186547,-0.707106781186548));
#14368=DIRECTION('ref_axis',(0.,0.707106781186548,0.707106781186547));
#14369=DIRECTION('',(0.,0.707106781186548,0.707106781186547));
#14370=DIRECTION('',(1.,0.,0.));
#14371=DIRECTION('',(0.,-0.707106781186548,-0.707106781186547));
#14372=DIRECTION('center_axis',(0.,0.,-1.));
#14373=DIRECTION('ref_axis',(0.,1.,0.));
#14374=DIRECTION('',(0.,1.,0.));
#14375=DIRECTION('',(1.,0.,0.));
#14376=DIRECTION('',(0.,-1.,0.));
#14377=DIRECTION('center_axis',(0.,-0.707106781186547,-0.707106781186548));
#14378=DIRECTION('ref_axis',(0.,0.707106781186548,-0.707106781186547));
#14379=DIRECTION('',(0.,0.707106781186548,-0.707106781186547));
#14380=DIRECTION('',(1.,0.,0.));
#14381=DIRECTION('',(0.,-0.707106781186548,0.707106781186547));
#14382=DIRECTION('center_axis',(0.,-1.,0.));
#14383=DIRECTION('ref_axis',(0.,0.,-1.));
#14384=DIRECTION('',(0.,0.,-1.));
#14385=DIRECTION('',(1.,0.,0.));
#14386=DIRECTION('',(0.,0.,1.));
#14387=DIRECTION('center_axis',(0.,0.,1.));
#14388=DIRECTION('ref_axis',(0.,-1.,0.));
#14389=DIRECTION('',(0.,-1.,0.));
#14390=DIRECTION('',(1.,0.,0.));
#14391=DIRECTION('',(0.,1.,0.));
#14392=DIRECTION('center_axis',(0.,-1.,0.));
#14393=DIRECTION('ref_axis',(0.,0.,-1.));
#14394=DIRECTION('',(0.,0.,-1.));
#14395=DIRECTION('',(-1.,0.,0.));
#14396=DIRECTION('',(0.,0.,1.));
#14397=DIRECTION('center_axis',(1.,0.,0.));
#14398=DIRECTION('ref_axis',(0.,0.,-1.));
#14399=DIRECTION('center_axis',(1.,0.,0.));
#14400=DIRECTION('ref_axis',(0.,0.,-1.));
#14401=DIRECTION('',(1.,0.,0.));
#14402=DIRECTION('center_axis',(-1.,0.,0.));
#14403=DIRECTION('ref_axis',(0.,0.,-1.));
#14404=DIRECTION('center_axis',(0.,1.,0.));
#14405=DIRECTION('ref_axis',(0.,0.,1.));
#14406=DIRECTION('',(0.,0.,1.));
#14407=DIRECTION('',(1.,0.,0.));
#14408=DIRECTION('',(0.,0.,1.));
#14409=DIRECTION('center_axis',(0.,1.,0.));
#14410=DIRECTION('ref_axis',(0.,0.,1.));
#14411=DIRECTION('',(0.,0.,1.));
#14412=DIRECTION('',(1.,0.,0.));
#14413=DIRECTION('',(0.,0.,1.));
#14414=DIRECTION('center_axis',(0.,0.,-1.));
#14415=DIRECTION('ref_axis',(0.,1.,0.));
#14416=DIRECTION('',(0.,1.,0.));
#14417=DIRECTION('',(0.,1.,0.));
#14418=DIRECTION('center_axis',(0.,0.,-1.));
#14419=DIRECTION('ref_axis',(0.,1.,0.));
#14420=DIRECTION('',(0.,1.,0.));
#14421=DIRECTION('',(1.,0.,0.));
#14422=DIRECTION('',(0.,1.,0.));
#14423=DIRECTION('center_axis',(0.,-1.,0.));
#14424=DIRECTION('ref_axis',(0.,0.,-1.));
#14425=DIRECTION('',(0.,0.,-1.));
#14426=DIRECTION('',(0.,0.,-1.));
#14427=DIRECTION('center_axis',(0.,-1.,0.));
#14428=DIRECTION('ref_axis',(0.,0.,-1.));
#14429=DIRECTION('',(0.,0.,-1.));
#14430=DIRECTION('',(1.,0.,0.));
#14431=DIRECTION('',(0.,0.,-1.));
#14432=DIRECTION('center_axis',(0.,0.,1.));
#14433=DIRECTION('ref_axis',(0.,-1.,0.));
#14434=DIRECTION('',(0.,-1.,0.));
#14435=DIRECTION('',(0.,-1.,0.));
#14436=DIRECTION('center_axis',(0.,0.,1.));
#14437=DIRECTION('ref_axis',(0.,-1.,0.));
#14438=DIRECTION('',(0.,-1.,0.));
#14439=DIRECTION('',(0.,-1.,0.));
#14440=DIRECTION('center_axis',(1.,0.,0.));
#14441=DIRECTION('ref_axis',(0.,0.,-1.));
#14442=DIRECTION('center_axis',(1.,0.,0.));
#14443=DIRECTION('ref_axis',(0.,0.,-1.));
#14444=DIRECTION('axis',(0.,0.,1.));
#14445=DIRECTION('refdir',(1.,0.,0.));
#14446=DIRECTION('center_axis',(0.,0.,1.));
#14447=DIRECTION('ref_axis',(1.,0.,0.));
#14448=DIRECTION('',(1.,0.,0.));
#14449=DIRECTION('',(0.,-1.,0.));
#14450=DIRECTION('',(-1.,0.,0.));
#14451=DIRECTION('',(0.,1.,0.));
#14452=DIRECTION('center_axis',(0.,1.,0.));
#14453=DIRECTION('ref_axis',(-1.,0.,0.));
#14454=DIRECTION('',(0.,0.,1.));
#14455=DIRECTION('',(-1.,0.,0.));
#14456=DIRECTION('',(0.,0.,1.));
#14457=DIRECTION('center_axis',(0.,0.,1.));
#14458=DIRECTION('ref_axis',(1.,0.,0.));
#14459=DIRECTION('',(0.,-1.,0.));
#14460=DIRECTION('',(1.,0.,0.));
#14461=DIRECTION('',(0.,1.,0.));
#14462=DIRECTION('center_axis',(0.,0.,-1.));
#14463=DIRECTION('ref_axis',(1.,0.,0.));
#14464=DIRECTION('center_axis',(-1.,0.,0.));
#14465=DIRECTION('ref_axis',(0.,-1.,0.));
#14466=DIRECTION('',(0.,0.,1.));
#14467=DIRECTION('',(0.,0.707106781186548,0.707106781186548));
#14468=DIRECTION('',(0.,-1.,0.));
#14469=DIRECTION('',(0.,0.707106781186548,-0.707106781186548));
#14470=DIRECTION('',(0.,0.,1.));
#14471=DIRECTION('',(0.,-1.,0.));
#14472=DIRECTION('',(0.,0.,1.));
#14473=DIRECTION('center_axis',(0.,-1.,0.));
#14474=DIRECTION('ref_axis',(1.,0.,0.));
#14475=DIRECTION('',(1.,0.,0.));
#14476=DIRECTION('',(0.,0.,1.));
#14477=DIRECTION('center_axis',(0.,0.,1.));
#14478=DIRECTION('ref_axis',(1.,0.,0.));
#14479=DIRECTION('',(-1.,0.,0.));
#14480=DIRECTION('',(0.,1.,0.));
#14481=DIRECTION('center_axis',(1.,0.,0.));
#14482=DIRECTION('ref_axis',(0.,1.,0.));
#14483=DIRECTION('',(0.,0.,1.));
#14484=DIRECTION('',(0.,-0.707106781186548,0.707106781186548));
#14485=DIRECTION('',(0.,1.,0.));
#14486=DIRECTION('',(0.,-0.707106781186548,-0.707106781186548));
#14487=DIRECTION('',(0.,0.,1.));
#14488=DIRECTION('center_axis',(0.,-1.,0.));
#14489=DIRECTION('ref_axis',(1.,0.,0.));
#14490=DIRECTION('',(-1.,0.,0.));
#14491=DIRECTION('center_axis',(0.,-0.707106781186548,-0.707106781186548));
#14492=DIRECTION('ref_axis',(-1.,0.,0.));
#14493=DIRECTION('',(1.,0.,0.));
#14494=DIRECTION('center_axis',(0.,0.707106781186548,0.707106781186548));
#14495=DIRECTION('ref_axis',(0.,0.707106781186547,-0.707106781186547));
#14496=DIRECTION('',(1.,0.,0.));
#14497=DIRECTION('center_axis',(0.,0.,1.));
#14498=DIRECTION('ref_axis',(1.,0.,0.));
#14499=DIRECTION('center_axis',(0.,0.,-1.));
#14500=DIRECTION('ref_axis',(1.,0.,0.));
#14501=DIRECTION('',(0.,0.,1.));
#14502=DIRECTION('center_axis',(0.,0.,-1.));
#14503=DIRECTION('ref_axis',(1.,0.,0.));
#14504=DIRECTION('center_axis',(0.,-0.707106781186548,0.707106781186548));
#14505=DIRECTION('ref_axis',(0.,0.707106781186547,0.707106781186547));
#14506=DIRECTION('center_axis',(0.,0.,-1.));
#14507=DIRECTION('ref_axis',(1.,0.,0.));
#14508=DIRECTION('center_axis',(0.,0.,1.));
#14509=DIRECTION('ref_axis',(1.,0.,0.));
#14510=DIRECTION('',(-1.,0.,0.));
#14511=DIRECTION('center_axis',(0.,0.,1.));
#14512=DIRECTION('ref_axis',(1.,0.,0.));
#14513=DIRECTION('',(-1.,0.,0.));
#14514=DIRECTION('center_axis',(0.,0.707106781186548,-0.707106781186548));
#14515=DIRECTION('ref_axis',(-1.,0.,0.));
#14516=DIRECTION('',(1.,0.,0.));
#14517=DIRECTION('center_axis',(0.,1.,0.));
#14518=DIRECTION('ref_axis',(-1.,0.,0.));
#14519=DIRECTION('axis',(0.,0.,1.));
#14520=DIRECTION('refdir',(1.,0.,0.));
#14521=DIRECTION('center_axis',(0.866025403784439,0.,-0.5));
#14522=DIRECTION('ref_axis',(0.5,0.,0.866025403784439));
#14523=DIRECTION('',(-0.5,0.,-0.866025403784439));
#14524=DIRECTION('',(0.,-1.,0.));
#14525=DIRECTION('',(0.5,0.,0.866025403784439));
#14526=DIRECTION('',(0.,-1.,0.));
#14527=DIRECTION('center_axis',(1.20185167898973E-16,0.,-1.));
#14528=DIRECTION('ref_axis',(1.,0.,1.20185167898973E-16));
#14529=DIRECTION('',(-1.,0.,-1.20185167898973E-16));
#14530=DIRECTION('',(0.,-1.,0.));
#14531=DIRECTION('',(1.,0.,1.20185167898973E-16));
#14532=DIRECTION('center_axis',(-0.866025403784439,0.,-0.5));
#14533=DIRECTION('ref_axis',(0.5,0.,-0.866025403784439));
#14534=DIRECTION('',(-0.5,0.,0.866025403784439));
#14535=DIRECTION('',(0.,-1.,0.));
#14536=DIRECTION('',(0.5,0.,-0.866025403784439));
#14537=DIRECTION('center_axis',(-0.866025403784439,0.,0.5));
#14538=DIRECTION('ref_axis',(-0.5,0.,-0.866025403784439));
#14539=DIRECTION('',(0.5,0.,0.866025403784439));
#14540=DIRECTION('',(0.,-1.,0.));
#14541=DIRECTION('',(-0.5,0.,-0.866025403784439));
#14542=DIRECTION('center_axis',(-2.40370335797945E-16,0.,1.));
#14543=DIRECTION('ref_axis',(-1.,0.,-2.40370335797945E-16));
#14544=DIRECTION('',(1.,0.,2.40370335797945E-16));
#14545=DIRECTION('',(0.,-1.,0.));
#14546=DIRECTION('',(-1.,0.,-2.40370335797945E-16));
#14547=DIRECTION('center_axis',(0.866025403784439,0.,0.5));
#14548=DIRECTION('ref_axis',(-0.5,0.,0.866025403784439));
#14549=DIRECTION('',(0.5,0.,-0.866025403784439));
#14550=DIRECTION('',(-0.5,0.,0.866025403784439));
#14551=DIRECTION('center_axis',(0.,1.,0.));
#14552=DIRECTION('ref_axis',(1.,0.,0.));
#14553=DIRECTION('center_axis',(0.,-1.,0.));
#14554=DIRECTION('ref_axis',(0.,0.,-1.));
#14555=DIRECTION('center_axis',(0.,1.,0.));
#14556=DIRECTION('ref_axis',(1.,0.,0.));
#14557=DIRECTION('center_axis',(0.,1.,0.));
#14558=DIRECTION('ref_axis',(1.,0.,0.));
#14559=DIRECTION('center_axis',(0.,1.,0.));
#14560=DIRECTION('ref_axis',(0.,0.,1.));
#14561=DIRECTION('center_axis',(0.,-1.,0.));
#14562=DIRECTION('ref_axis',(1.,0.,0.));
#14563=DIRECTION('center_axis',(0.,-1.,0.));
#14564=DIRECTION('ref_axis',(1.,0.,0.));
#14565=DIRECTION('center_axis',(0.,-1.,0.));
#14566=DIRECTION('ref_axis',(1.,0.,0.));
#14567=DIRECTION('',(0.707106781186548,0.707106781186547,8.65956056235493E-17));
#14568=DIRECTION('center_axis',(0.,-1.,0.));
#14569=DIRECTION('ref_axis',(1.,0.,0.));
#14570=DIRECTION('center_axis',(0.,-1.,0.));
#14571=DIRECTION('ref_axis',(1.,0.,0.));
#14572=DIRECTION('',(0.,1.,0.));
#14573=DIRECTION('center_axis',(0.,1.,0.));
#14574=DIRECTION('ref_axis',(1.,0.,0.));
#14575=DIRECTION('center_axis',(0.,-1.,0.));
#14576=DIRECTION('ref_axis',(1.,0.,0.));
#14577=DIRECTION('',(-0.707106781186547,0.707106781186548,-8.65956056235493E-17));
#14578=DIRECTION('center_axis',(0.,-1.,0.));
#14579=DIRECTION('ref_axis',(0.,0.,-1.));
#14580=DIRECTION('center_axis',(0.,-1.,0.));
#14581=DIRECTION('ref_axis',(1.,0.,0.));
#14582=DIRECTION('center_axis',(0.,1.,0.));
#14583=DIRECTION('ref_axis',(1.,0.,0.));
#14584=DIRECTION('center_axis',(0.,1.,0.));
#14585=DIRECTION('ref_axis',(1.,0.,0.));
#14586=DIRECTION('',(-0.447213595499958,0.894427190999916,-5.47678698264203E-17));
#14587=DIRECTION('center_axis',(0.,-1.,0.));
#14588=DIRECTION('ref_axis',(1.,0.,0.));
#14589=DIRECTION('',(0.,1.,0.));
#14590=DIRECTION('axis',(0.,0.,1.));
#14591=DIRECTION('refdir',(1.,0.,0.));
#14592=DIRECTION('center_axis',(0.,0.,1.));
#14593=DIRECTION('ref_axis',(1.,0.,0.));
#14594=DIRECTION('center_axis',(0.,0.,1.));
#14595=DIRECTION('ref_axis',(1.,0.,0.));
#14596=DIRECTION('',(0.,0.,1.));
#14597=DIRECTION('center_axis',(0.,0.,-1.));
#14598=DIRECTION('ref_axis',(1.,0.,0.));
#14599=DIRECTION('center_axis',(0.,0.,1.));
#14600=DIRECTION('ref_axis',(1.,0.,0.));
#14601=DIRECTION('center_axis',(0.,0.,1.));
#14602=DIRECTION('ref_axis',(1.,0.,0.));
#14603=DIRECTION('center_axis',(0.,0.,1.));
#14604=DIRECTION('ref_axis',(1.,0.,0.));
#14605=DIRECTION('center_axis',(0.,0.,1.));
#14606=DIRECTION('ref_axis',(1.,0.,0.));
#14607=DIRECTION('',(0.,0.,1.));
#14608=DIRECTION('center_axis',(0.,0.,-1.));
#14609=DIRECTION('ref_axis',(1.,0.,0.));
#14610=DIRECTION('center_axis',(0.,0.,1.));
#14611=DIRECTION('ref_axis',(1.,0.,0.));
#14612=DIRECTION('center_axis',(0.,0.,1.));
#14613=DIRECTION('ref_axis',(1.,0.,0.));
#14614=DIRECTION('center_axis',(0.,0.,1.));
#14615=DIRECTION('ref_axis',(1.,0.,0.));
#14616=DIRECTION('center_axis',(0.,0.,1.));
#14617=DIRECTION('ref_axis',(1.,0.,0.));
#14618=DIRECTION('',(0.,0.,1.));
#14619=DIRECTION('center_axis',(0.,0.,-1.));
#14620=DIRECTION('ref_axis',(1.,0.,0.));
#14621=DIRECTION('center_axis',(0.,0.,1.));
#14622=DIRECTION('ref_axis',(1.,0.,0.));
#14623=DIRECTION('center_axis',(0.,0.,1.));
#14624=DIRECTION('ref_axis',(1.,0.,0.));
#14625=DIRECTION('center_axis',(0.,0.,1.));
#14626=DIRECTION('ref_axis',(1.,0.,0.));
#14627=DIRECTION('center_axis',(0.,0.,1.));
#14628=DIRECTION('ref_axis',(1.,0.,0.));
#14629=DIRECTION('',(0.,0.,1.));
#14630=DIRECTION('center_axis',(0.,0.,-1.));
#14631=DIRECTION('ref_axis',(1.,0.,0.));
#14632=DIRECTION('center_axis',(0.,0.,1.));
#14633=DIRECTION('ref_axis',(1.,0.,0.));
#14634=DIRECTION('center_axis',(0.,0.,1.));
#14635=DIRECTION('ref_axis',(1.,0.,0.));
#14636=DIRECTION('center_axis',(0.,0.,1.));
#14637=DIRECTION('ref_axis',(1.,0.,0.));
#14638=DIRECTION('center_axis',(0.,0.,1.));
#14639=DIRECTION('ref_axis',(1.,0.,0.));
#14640=DIRECTION('',(0.,0.,1.));
#14641=DIRECTION('center_axis',(0.,0.,1.));
#14642=DIRECTION('ref_axis',(1.,0.,0.));
#14643=DIRECTION('center_axis',(0.,0.,1.));
#14644=DIRECTION('ref_axis',(1.,0.,0.));
#14645=DIRECTION('',(0.,0.,1.));
#14646=DIRECTION('center_axis',(0.,0.,1.));
#14647=DIRECTION('ref_axis',(1.,0.,0.));
#14648=DIRECTION('center_axis',(0.,0.,1.));
#14649=DIRECTION('ref_axis',(1.,0.,0.));
#14650=DIRECTION('',(0.,0.,1.));
#14651=DIRECTION('center_axis',(0.,0.,1.));
#14652=DIRECTION('ref_axis',(1.,0.,0.));
#14653=DIRECTION('center_axis',(0.,0.,1.));
#14654=DIRECTION('ref_axis',(1.,0.,0.));
#14655=DIRECTION('',(0.,0.,1.));
#14656=DIRECTION('center_axis',(0.,-0.56333682464151,0.826227342807548));
#14657=DIRECTION('ref_axis',(0.,-0.826227342807548,-0.56333682464151));
#14658=DIRECTION('',(0.,-0.826227342807548,-0.56333682464151));
#14659=DIRECTION('',(1.,0.,0.));
#14660=DIRECTION('',(0.,-0.826227342807548,-0.56333682464151));
#14661=DIRECTION('',(1.,0.,0.));
#14662=DIRECTION('center_axis',(0.,-1.,0.));
#14663=DIRECTION('ref_axis',(0.,0.,-1.));
#14664=DIRECTION('',(0.,0.,-1.));
#14665=DIRECTION('',(0.,0.,-1.));
#14666=DIRECTION('',(1.,0.,0.));
#14667=DIRECTION('center_axis',(0.,-0.56333682464151,-0.826227342807548));
#14668=DIRECTION('ref_axis',(0.,0.826227342807548,-0.56333682464151));
#14669=DIRECTION('',(0.,0.826227342807548,-0.56333682464151));
#14670=DIRECTION('',(0.,0.826227342807548,-0.56333682464151));
#14671=DIRECTION('',(1.,0.,0.));
#14672=DIRECTION('center_axis',(0.,-1.,0.));
#14673=DIRECTION('ref_axis',(0.,0.,-1.));
#14674=DIRECTION('',(0.,0.,-1.));
#14675=DIRECTION('',(0.,0.,-1.));
#14676=DIRECTION('',(1.,0.,0.));
#14677=DIRECTION('center_axis',(0.,0.,1.));
#14678=DIRECTION('ref_axis',(0.,-1.,0.));
#14679=DIRECTION('',(0.,-1.,0.));
#14680=DIRECTION('',(0.,-1.,0.));
#14681=DIRECTION('',(1.,0.,0.));
#14682=DIRECTION('center_axis',(0.,1.,0.));
#14683=DIRECTION('ref_axis',(0.,0.,1.));
#14684=DIRECTION('',(0.,0.,1.));
#14685=DIRECTION('',(0.,0.,1.));
#14686=DIRECTION('',(1.,0.,0.));
#14687=DIRECTION('center_axis',(0.,0.56333682464151,-0.826227342807548));
#14688=DIRECTION('ref_axis',(0.,0.826227342807548,0.56333682464151));
#14689=DIRECTION('',(0.,0.826227342807548,0.56333682464151));
#14690=DIRECTION('',(0.,0.826227342807548,0.56333682464151));
#14691=DIRECTION('',(1.,0.,0.));
#14692=DIRECTION('center_axis',(0.,1.,0.));
#14693=DIRECTION('ref_axis',(0.,0.,1.));
#14694=DIRECTION('',(0.,0.,1.));
#14695=DIRECTION('',(0.,0.,1.));
#14696=DIRECTION('',(1.,0.,0.));
#14697=DIRECTION('center_axis',(0.,0.56333682464151,0.826227342807548));
#14698=DIRECTION('ref_axis',(0.,-0.826227342807548,0.56333682464151));
#14699=DIRECTION('',(0.,-0.826227342807548,0.56333682464151));
#14700=DIRECTION('',(0.,-0.826227342807548,0.56333682464151));
#14701=DIRECTION('',(1.,0.,0.));
#14702=DIRECTION('center_axis',(0.,1.,0.));
#14703=DIRECTION('ref_axis',(0.,0.,1.));
#14704=DIRECTION('',(0.,0.,1.));
#14705=DIRECTION('',(0.,0.,1.));
#14706=DIRECTION('',(1.,0.,0.));
#14707=DIRECTION('center_axis',(0.,0.,-1.));
#14708=DIRECTION('ref_axis',(0.,1.,0.));
#14709=DIRECTION('',(0.,1.,0.));
#14710=DIRECTION('',(0.,1.,0.));
#14711=DIRECTION('',(1.,0.,0.));
#14712=DIRECTION('center_axis',(0.,-1.,0.));
#14713=DIRECTION('ref_axis',(0.,0.,-1.));
#14714=DIRECTION('',(0.,0.,-1.));
#14715=DIRECTION('',(0.,0.,-1.));
#14716=DIRECTION('center_axis',(1.,0.,0.));
#14717=DIRECTION('ref_axis',(0.,0.,-1.));
#14718=DIRECTION('center_axis',(1.,0.,0.));
#14719=DIRECTION('ref_axis',(0.,0.,-1.));
#14720=DIRECTION('axis',(0.,0.,1.));
#14721=DIRECTION('refdir',(1.,0.,0.));
#14722=DIRECTION('axis',(0.,0.,1.));
#14723=DIRECTION('refdir',(1.,0.,0.));
#14724=DIRECTION('center_axis',(0.,1.,0.));
#14725=DIRECTION('ref_axis',(1.,0.,0.));
#14726=DIRECTION('center_axis',(0.,1.,0.));
#14727=DIRECTION('ref_axis',(1.,0.,0.));
#14728=DIRECTION('',(0.,1.,0.));
#14729=DIRECTION('center_axis',(0.,1.,0.));
#14730=DIRECTION('ref_axis',(1.,0.,0.));
#14731=DIRECTION('center_axis',(0.,1.,0.));
#14732=DIRECTION('ref_axis',(1.,0.,0.));
#14733=DIRECTION('center_axis',(0.,1.,0.));
#14734=DIRECTION('ref_axis',(1.,0.,0.));
#14735=DIRECTION('center_axis',(0.,1.,0.));
#14736=DIRECTION('ref_axis',(1.,0.,0.));
#14737=DIRECTION('center_axis',(0.,1.,0.));
#14738=DIRECTION('ref_axis',(1.,0.,0.));
#14739=DIRECTION('center_axis',(0.,1.,0.));
#14740=DIRECTION('ref_axis',(1.,0.,0.));
#14741=DIRECTION('center_axis',(0.,1.,0.));
#14742=DIRECTION('ref_axis',(1.,0.,0.));
#14743=DIRECTION('center_axis',(0.,-1.,0.));
#14744=DIRECTION('ref_axis',(1.,0.,0.));
#14745=DIRECTION('center_axis',(0.,1.,0.));
#14746=DIRECTION('ref_axis',(1.,0.,0.));
#14747=DIRECTION('',(0.,-1.,0.));
#14748=DIRECTION('center_axis',(0.,1.,0.));
#14749=DIRECTION('ref_axis',(1.,0.,0.));
#14750=DIRECTION('',(0.,-1.,0.));
#14751=DIRECTION('center_axis',(0.,1.,0.));
#14752=DIRECTION('ref_axis',(1.,0.,0.));
#14753=DIRECTION('center_axis',(0.,1.,0.));
#14754=DIRECTION('ref_axis',(1.,0.,0.));
#14755=DIRECTION('center_axis',(0.,1.,0.));
#14756=DIRECTION('ref_axis',(1.,0.,0.));
#14757=DIRECTION('',(0.,-1.,0.));
#14758=DIRECTION('center_axis',(0.,1.,0.));
#14759=DIRECTION('ref_axis',(1.,0.,0.));
#14760=DIRECTION('center_axis',(0.,1.,0.));
#14761=DIRECTION('ref_axis',(1.,0.,0.));
#14762=DIRECTION('center_axis',(0.,1.,0.));
#14763=DIRECTION('ref_axis',(1.,0.,0.));
#14764=DIRECTION('center_axis',(0.,1.,0.));
#14765=DIRECTION('ref_axis',(1.,0.,0.));
#14766=DIRECTION('',(0.,-1.,0.));
#14767=DIRECTION('center_axis',(0.,1.,0.));
#14768=DIRECTION('ref_axis',(1.,0.,0.));
#14769=DIRECTION('center_axis',(0.,1.,0.));
#14770=DIRECTION('ref_axis',(1.,0.,0.));
#14771=DIRECTION('axis',(0.,0.,1.));
#14772=DIRECTION('refdir',(1.,0.,0.));
#14773=DIRECTION('center_axis',(0.,1.,0.));
#14774=DIRECTION('ref_axis',(1.,0.,0.));
#14775=DIRECTION('center_axis',(0.,1.,0.));
#14776=DIRECTION('ref_axis',(1.,0.,0.));
#14777=DIRECTION('',(0.,1.,0.));
#14778=DIRECTION('center_axis',(0.,-1.,0.));
#14779=DIRECTION('ref_axis',(1.,0.,0.));
#14780=DIRECTION('center_axis',(0.,1.,0.));
#14781=DIRECTION('ref_axis',(1.,0.,0.));
#14782=DIRECTION('center_axis',(0.,1.,0.));
#14783=DIRECTION('ref_axis',(1.,0.,0.));
#14784=DIRECTION('center_axis',(0.,1.,0.));
#14785=DIRECTION('ref_axis',(1.,0.,0.));
#14786=DIRECTION('',(0.,-1.,0.));
#14787=DIRECTION('center_axis',(0.,-1.,0.));
#14788=DIRECTION('ref_axis',(1.,0.,0.));
#14789=DIRECTION('center_axis',(0.,1.,0.));
#14790=DIRECTION('ref_axis',(1.,0.,0.));
#14791=DIRECTION('center_axis',(0.,1.,0.));
#14792=DIRECTION('ref_axis',(1.,0.,0.));
#14793=DIRECTION('',(0.,-1.,0.));
#14794=DIRECTION('center_axis',(0.,1.,0.));
#14795=DIRECTION('ref_axis',(1.,0.,0.));
#14796=DIRECTION('center_axis',(0.,1.,0.));
#14797=DIRECTION('ref_axis',(1.,0.,0.));
#14798=DIRECTION('center_axis',(0.,1.,0.));
#14799=DIRECTION('ref_axis',(1.,0.,0.));
#14800=DIRECTION('axis',(0.,0.,1.));
#14801=DIRECTION('refdir',(1.,0.,0.));
#14802=DIRECTION('center_axis',(0.,1.,0.));
#14803=DIRECTION('ref_axis',(1.,0.,0.));
#14804=DIRECTION('center_axis',(0.,-1.,0.));
#14805=DIRECTION('ref_axis',(1.,0.,0.));
#14806=DIRECTION('',(0.,-1.,0.));
#14807=DIRECTION('center_axis',(0.,-1.,0.));
#14808=DIRECTION('ref_axis',(1.,0.,0.));
#14809=DIRECTION('center_axis',(0.,1.,0.));
#14810=DIRECTION('ref_axis',(1.,0.,0.));
#14811=DIRECTION('center_axis',(0.,1.,0.));
#14812=DIRECTION('ref_axis',(1.,0.,0.));
#14813=DIRECTION('',(0.,-1.,0.));
#14814=DIRECTION('center_axis',(0.,1.,0.));
#14815=DIRECTION('ref_axis',(1.,0.,0.));
#14816=DIRECTION('center_axis',(0.,1.,0.));
#14817=DIRECTION('ref_axis',(1.,0.,0.));
#14818=DIRECTION('center_axis',(0.,1.,0.));
#14819=DIRECTION('ref_axis',(1.,0.,0.));
#14820=DIRECTION('axis',(0.,0.,1.));
#14821=DIRECTION('refdir',(1.,0.,0.));
#14822=DIRECTION('center_axis',(0.,0.,1.));
#14823=DIRECTION('ref_axis',(1.,0.,0.));
#14824=DIRECTION('center_axis',(0.,0.,1.));
#14825=DIRECTION('ref_axis',(1.,0.,0.));
#14826=DIRECTION('',(0.,0.,-1.));
#14827=DIRECTION('center_axis',(0.,0.,1.));
#14828=DIRECTION('ref_axis',(1.,0.,0.));
#14829=DIRECTION('center_axis',(0.,0.,1.));
#14830=DIRECTION('ref_axis',(1.,0.,0.));
#14831=DIRECTION('center_axis',(0.,0.,1.));
#14832=DIRECTION('ref_axis',(1.,0.,0.));
#14833=DIRECTION('axis',(0.,0.,1.));
#14834=DIRECTION('refdir',(1.,0.,0.));
#14835=DIRECTION('center_axis',(0.,0.,1.));
#14836=DIRECTION('ref_axis',(1.,0.,0.));
#14837=DIRECTION('center_axis',(0.,0.,1.));
#14838=DIRECTION('ref_axis',(1.,0.,0.));
#14839=DIRECTION('',(0.,0.,-1.));
#14840=DIRECTION('center_axis',(0.,0.,1.));
#14841=DIRECTION('ref_axis',(1.,0.,0.));
#14842=DIRECTION('center_axis',(0.,0.,1.));
#14843=DIRECTION('ref_axis',(1.,0.,0.));
#14844=DIRECTION('center_axis',(0.,0.,1.));
#14845=DIRECTION('ref_axis',(1.,0.,0.));
#14846=DIRECTION('axis',(0.,0.,1.));
#14847=DIRECTION('refdir',(1.,0.,0.));
#14848=DIRECTION('center_axis',(0.,1.,0.));
#14849=DIRECTION('ref_axis',(1.,0.,0.));
#14850=DIRECTION('center_axis',(0.,-1.,0.));
#14851=DIRECTION('ref_axis',(1.,0.,0.));
#14852=DIRECTION('',(0.,-1.,0.));
#14853=DIRECTION('center_axis',(0.,-1.,0.));
#14854=DIRECTION('ref_axis',(1.,0.,0.));
#14855=DIRECTION('center_axis',(0.,1.,0.));
#14856=DIRECTION('ref_axis',(1.,0.,0.));
#14857=DIRECTION('center_axis',(0.,1.,0.));
#14858=DIRECTION('ref_axis',(1.,0.,0.));
#14859=DIRECTION('',(0.,-1.,0.));
#14860=DIRECTION('center_axis',(0.,1.,0.));
#14861=DIRECTION('ref_axis',(1.,0.,0.));
#14862=DIRECTION('center_axis',(0.,1.,0.));
#14863=DIRECTION('ref_axis',(1.,0.,0.));
#14864=DIRECTION('center_axis',(0.,1.,0.));
#14865=DIRECTION('ref_axis',(1.,0.,0.));
#14866=DIRECTION('axis',(0.,0.,1.));
#14867=DIRECTION('refdir',(1.,0.,0.));
#14868=DIRECTION('axis',(0.,0.,1.));
#14869=DIRECTION('refdir',(1.,0.,0.));
#14870=DIRECTION('center_axis',(0.,1.,0.));
#14871=DIRECTION('ref_axis',(1.,0.,0.));
#14872=DIRECTION('center_axis',(0.,1.,0.));
#14873=DIRECTION('ref_axis',(1.,0.,0.));
#14874=DIRECTION('',(0.,1.,0.));
#14875=DIRECTION('center_axis',(0.,1.,0.));
#14876=DIRECTION('ref_axis',(1.,0.,0.));
#14877=DIRECTION('center_axis',(0.,1.,0.));
#14878=DIRECTION('ref_axis',(1.,0.,0.));
#14879=DIRECTION('center_axis',(0.,1.,0.));
#14880=DIRECTION('ref_axis',(1.,0.,0.));
#14881=DIRECTION('center_axis',(0.,1.,0.));
#14882=DIRECTION('ref_axis',(1.,0.,0.));
#14883=DIRECTION('center_axis',(0.,1.,0.));
#14884=DIRECTION('ref_axis',(1.,0.,0.));
#14885=DIRECTION('center_axis',(0.,1.,0.));
#14886=DIRECTION('ref_axis',(1.,0.,0.));
#14887=DIRECTION('center_axis',(0.,1.,0.));
#14888=DIRECTION('ref_axis',(1.,0.,0.));
#14889=DIRECTION('center_axis',(0.,-1.,0.));
#14890=DIRECTION('ref_axis',(1.,0.,0.));
#14891=DIRECTION('center_axis',(0.,1.,0.));
#14892=DIRECTION('ref_axis',(1.,0.,0.));
#14893=DIRECTION('',(0.,-1.,0.));
#14894=DIRECTION('center_axis',(0.,1.,0.));
#14895=DIRECTION('ref_axis',(1.,0.,0.));
#14896=DIRECTION('',(0.,-1.,0.));
#14897=DIRECTION('center_axis',(0.,1.,0.));
#14898=DIRECTION('ref_axis',(1.,0.,0.));
#14899=DIRECTION('center_axis',(0.,1.,0.));
#14900=DIRECTION('ref_axis',(1.,0.,0.));
#14901=DIRECTION('center_axis',(0.,1.,0.));
#14902=DIRECTION('ref_axis',(1.,0.,0.));
#14903=DIRECTION('',(0.,-1.,0.));
#14904=DIRECTION('center_axis',(0.,1.,0.));
#14905=DIRECTION('ref_axis',(1.,0.,0.));
#14906=DIRECTION('center_axis',(0.,1.,0.));
#14907=DIRECTION('ref_axis',(1.,0.,0.));
#14908=DIRECTION('center_axis',(0.,1.,0.));
#14909=DIRECTION('ref_axis',(1.,0.,0.));
#14910=DIRECTION('center_axis',(0.,1.,0.));
#14911=DIRECTION('ref_axis',(1.,0.,0.));
#14912=DIRECTION('',(0.,-1.,0.));
#14913=DIRECTION('center_axis',(0.,1.,0.));
#14914=DIRECTION('ref_axis',(1.,0.,0.));
#14915=DIRECTION('center_axis',(0.,1.,0.));
#14916=DIRECTION('ref_axis',(1.,0.,0.));
#14917=DIRECTION('axis',(0.,0.,1.));
#14918=DIRECTION('refdir',(1.,0.,0.));
#14919=DIRECTION('center_axis',(0.,1.,0.));
#14920=DIRECTION('ref_axis',(1.,0.,0.));
#14921=DIRECTION('center_axis',(0.,1.,0.));
#14922=DIRECTION('ref_axis',(1.,0.,0.));
#14923=DIRECTION('',(0.,1.,0.));
#14924=DIRECTION('center_axis',(0.,-1.,0.));
#14925=DIRECTION('ref_axis',(1.,0.,0.));
#14926=DIRECTION('center_axis',(0.,1.,0.));
#14927=DIRECTION('ref_axis',(1.,0.,0.));
#14928=DIRECTION('center_axis',(0.,1.,0.));
#14929=DIRECTION('ref_axis',(1.,0.,0.));
#14930=DIRECTION('center_axis',(0.,1.,0.));
#14931=DIRECTION('ref_axis',(1.,0.,0.));
#14932=DIRECTION('',(0.,-1.,0.));
#14933=DIRECTION('center_axis',(0.,-1.,0.));
#14934=DIRECTION('ref_axis',(1.,0.,0.));
#14935=DIRECTION('center_axis',(0.,1.,0.));
#14936=DIRECTION('ref_axis',(1.,0.,0.));
#14937=DIRECTION('center_axis',(0.,1.,0.));
#14938=DIRECTION('ref_axis',(1.,0.,0.));
#14939=DIRECTION('',(0.,-1.,0.));
#14940=DIRECTION('center_axis',(0.,1.,0.));
#14941=DIRECTION('ref_axis',(1.,0.,0.));
#14942=DIRECTION('center_axis',(0.,1.,0.));
#14943=DIRECTION('ref_axis',(1.,0.,0.));
#14944=DIRECTION('center_axis',(0.,1.,0.));
#14945=DIRECTION('ref_axis',(1.,0.,0.));
#14946=DIRECTION('axis',(0.,0.,1.));
#14947=DIRECTION('refdir',(1.,0.,0.));
#14948=DIRECTION('center_axis',(0.,1.,0.));
#14949=DIRECTION('ref_axis',(1.,0.,0.));
#14950=DIRECTION('center_axis',(0.,-1.,0.));
#14951=DIRECTION('ref_axis',(1.,0.,0.));
#14952=DIRECTION('',(0.,-1.,0.));
#14953=DIRECTION('center_axis',(0.,-1.,0.));
#14954=DIRECTION('ref_axis',(1.,0.,0.));
#14955=DIRECTION('center_axis',(0.,1.,0.));
#14956=DIRECTION('ref_axis',(1.,0.,0.));
#14957=DIRECTION('center_axis',(0.,1.,0.));
#14958=DIRECTION('ref_axis',(1.,0.,0.));
#14959=DIRECTION('',(0.,-1.,0.));
#14960=DIRECTION('center_axis',(0.,1.,0.));
#14961=DIRECTION('ref_axis',(1.,0.,0.));
#14962=DIRECTION('center_axis',(0.,1.,0.));
#14963=DIRECTION('ref_axis',(1.,0.,0.));
#14964=DIRECTION('center_axis',(0.,1.,0.));
#14965=DIRECTION('ref_axis',(1.,0.,0.));
#14966=DIRECTION('axis',(0.,0.,1.));
#14967=DIRECTION('refdir',(1.,0.,0.));
#14968=DIRECTION('center_axis',(0.,0.,1.));
#14969=DIRECTION('ref_axis',(1.,0.,0.));
#14970=DIRECTION('center_axis',(0.,0.,1.));
#14971=DIRECTION('ref_axis',(1.,0.,0.));
#14972=DIRECTION('',(0.,0.,-1.));
#14973=DIRECTION('center_axis',(0.,0.,1.));
#14974=DIRECTION('ref_axis',(1.,0.,0.));
#14975=DIRECTION('center_axis',(0.,0.,1.));
#14976=DIRECTION('ref_axis',(1.,0.,0.));
#14977=DIRECTION('center_axis',(0.,0.,1.));
#14978=DIRECTION('ref_axis',(1.,0.,0.));
#14979=DIRECTION('axis',(0.,0.,1.));
#14980=DIRECTION('refdir',(1.,0.,0.));
#14981=DIRECTION('center_axis',(0.,0.,1.));
#14982=DIRECTION('ref_axis',(1.,0.,0.));
#14983=DIRECTION('center_axis',(0.,0.,1.));
#14984=DIRECTION('ref_axis',(1.,0.,0.));
#14985=DIRECTION('',(0.,0.,-1.));
#14986=DIRECTION('center_axis',(0.,0.,1.));
#14987=DIRECTION('ref_axis',(1.,0.,0.));
#14988=DIRECTION('center_axis',(0.,0.,1.));
#14989=DIRECTION('ref_axis',(1.,0.,0.));
#14990=DIRECTION('center_axis',(0.,0.,1.));
#14991=DIRECTION('ref_axis',(1.,0.,0.));
#14992=DIRECTION('axis',(0.,0.,1.));
#14993=DIRECTION('refdir',(1.,0.,0.));
#14994=DIRECTION('center_axis',(0.,1.,0.));
#14995=DIRECTION('ref_axis',(1.,0.,0.));
#14996=DIRECTION('center_axis',(0.,-1.,0.));
#14997=DIRECTION('ref_axis',(1.,0.,0.));
#14998=DIRECTION('',(0.,-1.,0.));
#14999=DIRECTION('center_axis',(0.,-1.,0.));
#15000=DIRECTION('ref_axis',(1.,0.,0.));
#15001=DIRECTION('center_axis',(0.,1.,0.));
#15002=DIRECTION('ref_axis',(1.,0.,0.));
#15003=DIRECTION('center_axis',(0.,1.,0.));
#15004=DIRECTION('ref_axis',(1.,0.,0.));
#15005=DIRECTION('',(0.,-1.,0.));
#15006=DIRECTION('center_axis',(0.,1.,0.));
#15007=DIRECTION('ref_axis',(1.,0.,0.));
#15008=DIRECTION('center_axis',(0.,1.,0.));
#15009=DIRECTION('ref_axis',(1.,0.,0.));
#15010=DIRECTION('center_axis',(0.,1.,0.));
#15011=DIRECTION('ref_axis',(1.,0.,0.));
#15012=DIRECTION('axis',(0.,0.,1.));
#15013=DIRECTION('refdir',(1.,0.,0.));
#15014=DIRECTION('center_axis',(1.,0.,6.12323399573677E-17));
#15015=DIRECTION('ref_axis',(6.12323399573677E-17,0.,-1.));
#15016=DIRECTION('',(1.,0.,6.12323399573677E-17));
#15017=DIRECTION('center_axis',(1.,0.,6.12323399573677E-17));
#15018=DIRECTION('ref_axis',(6.12323399573677E-17,0.,-1.));
#15019=DIRECTION('',(1.,0.,6.12323399573677E-17));
#15020=DIRECTION('center_axis',(0.,-1.,0.));
#15021=DIRECTION('ref_axis',(1.,0.,0.));
#15022=DIRECTION('center_axis',(0.,-1.,0.));
#15023=DIRECTION('ref_axis',(1.,0.,0.));
#15024=DIRECTION('',(0.,1.,0.));
#15025=DIRECTION('',(0.,1.,0.));
#15026=DIRECTION('center_axis',(0.,1.,0.));
#15027=DIRECTION('ref_axis',(1.,0.,0.));
#15028=DIRECTION('center_axis',(0.,0.,1.));
#15029=DIRECTION('ref_axis',(1.,0.,0.));
#15030=DIRECTION('',(0.,0.,1.));
#15031=DIRECTION('center_axis',(0.,0.,1.));
#15032=DIRECTION('ref_axis',(1.,0.,0.));
#15033=DIRECTION('',(0.,0.,1.));
#15034=DIRECTION('center_axis',(0.,1.,0.));
#15035=DIRECTION('ref_axis',(1.,0.,0.));
#15036=DIRECTION('center_axis',(0.,1.,0.));
#15037=DIRECTION('ref_axis',(1.,0.,0.));
#15038=DIRECTION('',(0.,1.,0.));
#15039=DIRECTION('',(0.,1.,0.));
#15040=DIRECTION('center_axis',(0.,-1.,0.));
#15041=DIRECTION('ref_axis',(1.,0.,0.));
#15042=DIRECTION('center_axis',(0.,1.,0.));
#15043=DIRECTION('ref_axis',(1.,0.,0.));
#15044=DIRECTION('center_axis',(0.,1.,0.));
#15045=DIRECTION('ref_axis',(1.,0.,0.));
#15046=DIRECTION('center_axis',(0.,1.,0.));
#15047=DIRECTION('ref_axis',(1.,0.,0.));
#15048=DIRECTION('center_axis',(0.,1.,0.));
#15049=DIRECTION('ref_axis',(0.951056516295154,0.,0.309016994374948));
#15050=DIRECTION('center_axis',(0.,1.,0.));
#15051=DIRECTION('ref_axis',(1.,0.,0.));
#15052=DIRECTION('center_axis',(0.,1.,0.));
#15053=DIRECTION('ref_axis',(0.809016994374947,0.,0.587785252292473));
#15054=DIRECTION('center_axis',(0.,1.,0.));
#15055=DIRECTION('ref_axis',(1.,0.,0.));
#15056=DIRECTION('center_axis',(0.,1.,0.));
#15057=DIRECTION('ref_axis',(0.587785252292473,0.,0.809016994374948));
#15058=DIRECTION('center_axis',(0.,1.,0.));
#15059=DIRECTION('ref_axis',(1.,0.,0.));
#15060=DIRECTION('center_axis',(0.,1.,0.));
#15061=DIRECTION('ref_axis',(0.309016994374947,0.,0.951056516295154));
#15062=DIRECTION('center_axis',(0.,1.,0.));
#15063=DIRECTION('ref_axis',(1.,0.,0.));
#15064=DIRECTION('center_axis',(0.,1.,0.));
#15065=DIRECTION('ref_axis',(-1.83697019872103E-16,0.,1.));
#15066=DIRECTION('center_axis',(0.,1.,0.));
#15067=DIRECTION('ref_axis',(1.,0.,0.));
#15068=DIRECTION('center_axis',(0.,1.,0.));
#15069=DIRECTION('ref_axis',(-0.309016994374948,0.,0.951056516295154));
#15070=DIRECTION('center_axis',(0.,1.,0.));
#15071=DIRECTION('ref_axis',(1.,0.,0.));
#15072=DIRECTION('center_axis',(0.,1.,0.));
#15073=DIRECTION('ref_axis',(-0.587785252292473,0.,0.809016994374947));
#15074=DIRECTION('center_axis',(0.,1.,0.));
#15075=DIRECTION('ref_axis',(1.,0.,0.));
#15076=DIRECTION('center_axis',(0.,1.,0.));
#15077=DIRECTION('ref_axis',(-0.809016994374947,0.,0.587785252292473));
#15078=DIRECTION('center_axis',(0.,1.,0.));
#15079=DIRECTION('ref_axis',(1.,0.,0.));
#15080=DIRECTION('center_axis',(0.,1.,0.));
#15081=DIRECTION('ref_axis',(-0.951056516295154,0.,0.309016994374947));
#15082=DIRECTION('center_axis',(0.,1.,0.));
#15083=DIRECTION('ref_axis',(1.,0.,0.));
#15084=DIRECTION('center_axis',(0.,1.,0.));
#15085=DIRECTION('ref_axis',(-1.,0.,-1.22464679914735E-16));
#15086=DIRECTION('center_axis',(0.,1.,0.));
#15087=DIRECTION('ref_axis',(1.,0.,0.));
#15088=DIRECTION('center_axis',(0.,1.,0.));
#15089=DIRECTION('ref_axis',(-0.951056516295154,0.,-0.309016994374948));
#15090=DIRECTION('center_axis',(0.,1.,0.));
#15091=DIRECTION('ref_axis',(1.,0.,0.));
#15092=DIRECTION('center_axis',(0.,1.,0.));
#15093=DIRECTION('ref_axis',(-0.809016994374947,0.,-0.587785252292473));
#15094=DIRECTION('center_axis',(0.,1.,0.));
#15095=DIRECTION('ref_axis',(1.,0.,0.));
#15096=DIRECTION('center_axis',(0.,1.,0.));
#15097=DIRECTION('ref_axis',(-0.587785252292473,0.,-0.809016994374948));
#15098=DIRECTION('center_axis',(0.,1.,0.));
#15099=DIRECTION('ref_axis',(1.,0.,0.));
#15100=DIRECTION('center_axis',(0.,1.,0.));
#15101=DIRECTION('ref_axis',(-0.309016994374947,0.,-0.951056516295154));
#15102=DIRECTION('center_axis',(0.,1.,0.));
#15103=DIRECTION('ref_axis',(1.,0.,0.));
#15104=DIRECTION('center_axis',(0.,1.,0.));
#15105=DIRECTION('ref_axis',(6.12323399573677E-17,0.,-1.));
#15106=DIRECTION('center_axis',(0.,1.,0.));
#15107=DIRECTION('ref_axis',(1.,0.,0.));
#15108=DIRECTION('center_axis',(0.,1.,0.));
#15109=DIRECTION('ref_axis',(0.309016994374947,0.,-0.951056516295154));
#15110=DIRECTION('center_axis',(0.,1.,0.));
#15111=DIRECTION('ref_axis',(1.,0.,0.));
#15112=DIRECTION('center_axis',(0.,1.,0.));
#15113=DIRECTION('ref_axis',(0.587785252292473,0.,-0.809016994374947));
#15114=DIRECTION('center_axis',(0.,1.,0.));
#15115=DIRECTION('ref_axis',(1.,0.,0.));
#15116=DIRECTION('center_axis',(0.,1.,0.));
#15117=DIRECTION('ref_axis',(0.809016994374947,0.,-0.587785252292473));
#15118=DIRECTION('center_axis',(0.,1.,0.));
#15119=DIRECTION('ref_axis',(1.,0.,0.));
#15120=DIRECTION('center_axis',(0.,1.,0.));
#15121=DIRECTION('ref_axis',(0.951056516295154,0.,-0.309016994374947));
#15122=DIRECTION('center_axis',(0.,1.,0.));
#15123=DIRECTION('ref_axis',(1.,0.,0.));
#15124=DIRECTION('center_axis',(0.,1.,0.));
#15125=DIRECTION('ref_axis',(1.,0.,0.));
#15126=DIRECTION('center_axis',(0.,1.,0.));
#15127=DIRECTION('ref_axis',(1.,0.,0.));
#15128=DIRECTION('center_axis',(0.,-1.,0.));
#15129=DIRECTION('ref_axis',(1.,0.,0.));
#15130=DIRECTION('center_axis',(0.,-1.,0.));
#15131=DIRECTION('ref_axis',(1.,0.,0.));
#15132=DIRECTION('',(0.,1.,0.));
#15133=DIRECTION('center_axis',(0.,1.,0.));
#15134=DIRECTION('ref_axis',(1.,0.,0.));
#15135=DIRECTION('center_axis',(0.,1.,0.));
#15136=DIRECTION('ref_axis',(1.,0.,0.));
#15137=DIRECTION('center_axis',(0.,1.,0.));
#15138=DIRECTION('ref_axis',(1.,0.,0.));
#15139=DIRECTION('center_axis',(0.,-1.,0.));
#15140=DIRECTION('ref_axis',(0.951056516295154,0.,0.309016994374948));
#15141=DIRECTION('center_axis',(0.,1.,0.));
#15142=DIRECTION('ref_axis',(1.,0.,0.));
#15143=DIRECTION('center_axis',(0.,-1.,0.));
#15144=DIRECTION('ref_axis',(1.,0.,0.));
#15145=DIRECTION('center_axis',(0.,1.,0.));
#15146=DIRECTION('ref_axis',(1.,0.,0.));
#15147=DIRECTION('center_axis',(0.,-1.,0.));
#15148=DIRECTION('ref_axis',(0.951056516295154,0.,-0.309016994374947));
#15149=DIRECTION('center_axis',(0.,1.,0.));
#15150=DIRECTION('ref_axis',(1.,0.,0.));
#15151=DIRECTION('center_axis',(0.,-1.,0.));
#15152=DIRECTION('ref_axis',(0.809016994374947,0.,-0.587785252292473));
#15153=DIRECTION('center_axis',(0.,1.,0.));
#15154=DIRECTION('ref_axis',(1.,0.,0.));
#15155=DIRECTION('center_axis',(0.,-1.,0.));
#15156=DIRECTION('ref_axis',(0.587785252292473,0.,-0.809016994374947));
#15157=DIRECTION('center_axis',(0.,1.,0.));
#15158=DIRECTION('ref_axis',(1.,0.,0.));
#15159=DIRECTION('center_axis',(0.,-1.,0.));
#15160=DIRECTION('ref_axis',(0.309016994374947,0.,-0.951056516295154));
#15161=DIRECTION('center_axis',(0.,1.,0.));
#15162=DIRECTION('ref_axis',(1.,0.,0.));
#15163=DIRECTION('center_axis',(0.,-1.,0.));
#15164=DIRECTION('ref_axis',(6.12323399573677E-17,0.,-1.));
#15165=DIRECTION('center_axis',(0.,1.,0.));
#15166=DIRECTION('ref_axis',(1.,0.,0.));
#15167=DIRECTION('center_axis',(0.,-1.,0.));
#15168=DIRECTION('ref_axis',(-0.309016994374947,0.,-0.951056516295154));
#15169=DIRECTION('center_axis',(0.,1.,0.));
#15170=DIRECTION('ref_axis',(1.,0.,0.));
#15171=DIRECTION('center_axis',(0.,-1.,0.));
#15172=DIRECTION('ref_axis',(-0.587785252292473,0.,-0.809016994374948));
#15173=DIRECTION('center_axis',(0.,1.,0.));
#15174=DIRECTION('ref_axis',(1.,0.,0.));
#15175=DIRECTION('center_axis',(0.,-1.,0.));
#15176=DIRECTION('ref_axis',(-0.809016994374947,0.,-0.587785252292473));
#15177=DIRECTION('center_axis',(0.,1.,0.));
#15178=DIRECTION('ref_axis',(1.,0.,0.));
#15179=DIRECTION('center_axis',(0.,-1.,0.));
#15180=DIRECTION('ref_axis',(-0.951056516295154,0.,-0.309016994374948));
#15181=DIRECTION('center_axis',(0.,1.,0.));
#15182=DIRECTION('ref_axis',(1.,0.,0.));
#15183=DIRECTION('center_axis',(0.,-1.,0.));
#15184=DIRECTION('ref_axis',(-1.,0.,-1.22464679914735E-16));
#15185=DIRECTION('center_axis',(0.,1.,0.));
#15186=DIRECTION('ref_axis',(1.,0.,0.));
#15187=DIRECTION('center_axis',(0.,-1.,0.));
#15188=DIRECTION('ref_axis',(-0.951056516295154,0.,0.309016994374947));
#15189=DIRECTION('center_axis',(0.,1.,0.));
#15190=DIRECTION('ref_axis',(1.,0.,0.));
#15191=DIRECTION('center_axis',(0.,-1.,0.));
#15192=DIRECTION('ref_axis',(-0.809016994374947,0.,0.587785252292473));
#15193=DIRECTION('center_axis',(0.,1.,0.));
#15194=DIRECTION('ref_axis',(1.,0.,0.));
#15195=DIRECTION('center_axis',(0.,-1.,0.));
#15196=DIRECTION('ref_axis',(-0.587785252292473,0.,0.809016994374947));
#15197=DIRECTION('center_axis',(0.,1.,0.));
#15198=DIRECTION('ref_axis',(1.,0.,0.));
#15199=DIRECTION('center_axis',(0.,-1.,0.));
#15200=DIRECTION('ref_axis',(-0.309016994374948,0.,0.951056516295154));
#15201=DIRECTION('center_axis',(0.,1.,0.));
#15202=DIRECTION('ref_axis',(1.,0.,0.));
#15203=DIRECTION('center_axis',(0.,-1.,0.));
#15204=DIRECTION('ref_axis',(-1.83697019872103E-16,0.,1.));
#15205=DIRECTION('center_axis',(0.,1.,0.));
#15206=DIRECTION('ref_axis',(1.,0.,0.));
#15207=DIRECTION('center_axis',(0.,-1.,0.));
#15208=DIRECTION('ref_axis',(0.309016994374947,0.,0.951056516295154));
#15209=DIRECTION('center_axis',(0.,1.,0.));
#15210=DIRECTION('ref_axis',(1.,0.,0.));
#15211=DIRECTION('center_axis',(0.,-1.,0.));
#15212=DIRECTION('ref_axis',(0.587785252292473,0.,0.809016994374948));
#15213=DIRECTION('center_axis',(0.,1.,0.));
#15214=DIRECTION('ref_axis',(1.,0.,0.));
#15215=DIRECTION('center_axis',(0.,-1.,0.));
#15216=DIRECTION('ref_axis',(0.809016994374947,0.,0.587785252292473));
#15217=DIRECTION('center_axis',(0.,1.,0.));
#15218=DIRECTION('ref_axis',(1.,0.,0.));
#15219=DIRECTION('center_axis',(0.,1.,0.));
#15220=DIRECTION('ref_axis',(1.,0.,0.));
#15221=DIRECTION('center_axis',(0.,1.,0.));
#15222=DIRECTION('ref_axis',(1.,0.,0.));
#15223=DIRECTION('',(0.,-1.,0.));
#15224=DIRECTION('center_axis',(0.,1.,0.));
#15225=DIRECTION('ref_axis',(1.,0.,0.));
#15226=DIRECTION('center_axis',(0.,1.,0.));
#15227=DIRECTION('ref_axis',(-0.951056516295153,0.,-0.309016994374948));
#15228=DIRECTION('',(0.,-1.,0.));
#15229=DIRECTION('',(0.,1.,0.));
#15230=DIRECTION('center_axis',(0.,1.,0.));
#15231=DIRECTION('ref_axis',(1.,0.,0.));
#15232=DIRECTION('',(0.,-1.,0.));
#15233=DIRECTION('center_axis',(0.,1.,0.));
#15234=DIRECTION('ref_axis',(-0.809016994374947,0.,-0.587785252292473));
#15235=DIRECTION('',(0.,1.,0.));
#15236=DIRECTION('center_axis',(0.,1.,0.));
#15237=DIRECTION('ref_axis',(1.,0.,0.));
#15238=DIRECTION('',(0.,-1.,0.));
#15239=DIRECTION('center_axis',(0.,1.,0.));
#15240=DIRECTION('ref_axis',(-0.587785252292473,0.,-0.809016994374947));
#15241=DIRECTION('',(0.,1.,0.));
#15242=DIRECTION('center_axis',(0.,1.,0.));
#15243=DIRECTION('ref_axis',(1.,0.,0.));
#15244=DIRECTION('',(0.,-1.,0.));
#15245=DIRECTION('center_axis',(0.,1.,0.));
#15246=DIRECTION('ref_axis',(-0.309016994374947,0.,-0.951056516295154));
#15247=DIRECTION('',(0.,1.,0.));
#15248=DIRECTION('center_axis',(0.,1.,0.));
#15249=DIRECTION('ref_axis',(1.,0.,0.));
#15250=DIRECTION('',(0.,-1.,0.));
#15251=DIRECTION('center_axis',(0.,1.,0.));
#15252=DIRECTION('ref_axis',(-1.37927510063224E-16,0.,-1.));
#15253=DIRECTION('',(0.,1.,0.));
#15254=DIRECTION('center_axis',(0.,1.,0.));
#15255=DIRECTION('ref_axis',(1.,0.,0.));
#15256=DIRECTION('',(0.,-1.,0.));
#15257=DIRECTION('center_axis',(0.,1.,0.));
#15258=DIRECTION('ref_axis',(0.309016994374948,0.,-0.951056516295154));
#15259=DIRECTION('',(0.,1.,0.));
#15260=DIRECTION('center_axis',(0.,1.,0.));
#15261=DIRECTION('ref_axis',(1.,0.,0.));
#15262=DIRECTION('',(0.,-1.,0.));
#15263=DIRECTION('center_axis',(0.,1.,0.));
#15264=DIRECTION('ref_axis',(0.587785252292473,0.,-0.809016994374948));
#15265=DIRECTION('',(0.,1.,0.));
#15266=DIRECTION('center_axis',(0.,1.,0.));
#15267=DIRECTION('ref_axis',(1.,0.,0.));
#15268=DIRECTION('',(0.,-1.,0.));
#15269=DIRECTION('center_axis',(0.,1.,0.));
#15270=DIRECTION('ref_axis',(0.809016994374948,0.,-0.587785252292473));
#15271=DIRECTION('',(0.,1.,0.));
#15272=DIRECTION('center_axis',(0.,1.,0.));
#15273=DIRECTION('ref_axis',(1.,0.,0.));
#15274=DIRECTION('',(0.,-1.,0.));
#15275=DIRECTION('center_axis',(0.,1.,0.));
#15276=DIRECTION('ref_axis',(0.951056516295154,0.,-0.309016994374947));
#15277=DIRECTION('',(0.,1.,0.));
#15278=DIRECTION('center_axis',(0.,1.,0.));
#15279=DIRECTION('ref_axis',(1.,0.,0.));
#15280=DIRECTION('',(0.,-1.,0.));
#15281=DIRECTION('center_axis',(0.,1.,0.));
#15282=DIRECTION('ref_axis',(1.,0.,-1.99159850020592E-16));
#15283=DIRECTION('',(0.,1.,0.));
#15284=DIRECTION('center_axis',(0.,1.,0.));
#15285=DIRECTION('ref_axis',(1.,0.,0.));
#15286=DIRECTION('',(0.,-1.,0.));
#15287=DIRECTION('center_axis',(0.,1.,0.));
#15288=DIRECTION('ref_axis',(0.951056516295154,0.,0.309016994374948));
#15289=DIRECTION('',(0.,1.,0.));
#15290=DIRECTION('center_axis',(0.,1.,0.));
#15291=DIRECTION('ref_axis',(1.,0.,0.));
#15292=DIRECTION('',(0.,-1.,0.));
#15293=DIRECTION('center_axis',(0.,1.,0.));
#15294=DIRECTION('ref_axis',(0.809016994374948,0.,0.587785252292473));
#15295=DIRECTION('',(0.,1.,0.));
#15296=DIRECTION('center_axis',(0.,1.,0.));
#15297=DIRECTION('ref_axis',(1.,0.,0.));
#15298=DIRECTION('',(0.,-1.,0.));
#15299=DIRECTION('center_axis',(0.,1.,0.));
#15300=DIRECTION('ref_axis',(0.587785252292473,0.,0.809016994374948));
#15301=DIRECTION('',(0.,1.,0.));
#15302=DIRECTION('center_axis',(0.,1.,0.));
#15303=DIRECTION('ref_axis',(1.,0.,0.));
#15304=DIRECTION('',(0.,-1.,0.));
#15305=DIRECTION('center_axis',(0.,1.,0.));
#15306=DIRECTION('ref_axis',(0.309016994374947,0.,0.951056516295154));
#15307=DIRECTION('',(0.,1.,0.));
#15308=DIRECTION('center_axis',(0.,1.,0.));
#15309=DIRECTION('ref_axis',(1.,0.,0.));
#15310=DIRECTION('',(0.,-1.,0.));
#15311=DIRECTION('center_axis',(0.,1.,0.));
#15312=DIRECTION('ref_axis',(2.6039218997796E-16,0.,1.));
#15313=DIRECTION('',(0.,1.,0.));
#15314=DIRECTION('center_axis',(0.,1.,0.));
#15315=DIRECTION('ref_axis',(1.,0.,0.));
#15316=DIRECTION('',(0.,-1.,0.));
#15317=DIRECTION('center_axis',(0.,1.,0.));
#15318=DIRECTION('ref_axis',(-0.309016994374948,0.,0.951056516295153));
#15319=DIRECTION('',(0.,1.,0.));
#15320=DIRECTION('center_axis',(0.,1.,0.));
#15321=DIRECTION('ref_axis',(1.,0.,0.));
#15322=DIRECTION('',(0.,-1.,0.));
#15323=DIRECTION('center_axis',(0.,1.,0.));
#15324=DIRECTION('ref_axis',(-0.587785252292474,0.,0.809016994374947));
#15325=DIRECTION('',(0.,1.,0.));
#15326=DIRECTION('center_axis',(0.,1.,0.));
#15327=DIRECTION('ref_axis',(1.,0.,0.));
#15328=DIRECTION('',(0.,-1.,0.));
#15329=DIRECTION('center_axis',(0.,1.,0.));
#15330=DIRECTION('ref_axis',(-0.809016994374948,0.,0.587785252292473));
#15331=DIRECTION('',(0.,1.,0.));
#15332=DIRECTION('center_axis',(0.,1.,0.));
#15333=DIRECTION('ref_axis',(1.,0.,0.));
#15334=DIRECTION('',(0.,-1.,0.));
#15335=DIRECTION('center_axis',(0.,1.,0.));
#15336=DIRECTION('ref_axis',(-0.951056516295154,0.,0.309016994374948));
#15337=DIRECTION('',(0.,1.,0.));
#15338=DIRECTION('center_axis',(0.,1.,0.));
#15339=DIRECTION('ref_axis',(1.,0.,0.));
#15340=DIRECTION('',(0.,1.,0.));
#15341=DIRECTION('center_axis',(0.,1.,0.));
#15342=DIRECTION('ref_axis',(-1.,0.,-1.22464679914735E-16));
#15343=DIRECTION('',(0.,-1.,0.));
#15344=DIRECTION('center_axis',(0.,1.,0.));
#15345=DIRECTION('ref_axis',(1.,0.,0.));
#15346=DIRECTION('axis',(0.,0.,1.));
#15347=DIRECTION('refdir',(1.,0.,0.));
#15348=DIRECTION('axis',(0.,0.,1.));
#15349=DIRECTION('refdir',(1.,0.,0.));
#15350=DIRECTION('center_axis',(0.,0.,1.));
#15351=DIRECTION('ref_axis',(1.,0.,0.));
#15352=DIRECTION('center_axis',(0.,0.,1.));
#15353=DIRECTION('ref_axis',(1.,0.,0.));
#15354=DIRECTION('',(0.,0.,1.));
#15355=DIRECTION('center_axis',(0.,0.,1.));
#15356=DIRECTION('ref_axis',(1.,0.,0.));
#15357=DIRECTION('center_axis',(0.,0.,1.));
#15358=DIRECTION('ref_axis',(1.,0.,0.));
#15359=DIRECTION('center_axis',(0.,0.,-1.));
#15360=DIRECTION('ref_axis',(1.,0.,0.));
#15361=DIRECTION('center_axis',(0.,0.,1.));
#15362=DIRECTION('ref_axis',(1.,0.,0.));
#15363=DIRECTION('center_axis',(0.,0.,1.));
#15364=DIRECTION('ref_axis',(1.,0.,0.));
#15365=DIRECTION('',(0.,0.,1.));
#15366=DIRECTION('center_axis',(0.,0.,1.));
#15367=DIRECTION('ref_axis',(1.,0.,0.));
#15368=DIRECTION('center_axis',(0.,0.,1.));
#15369=DIRECTION('ref_axis',(1.,0.,0.));
#15370=DIRECTION('center_axis',(0.,0.,-1.));
#15371=DIRECTION('ref_axis',(1.,0.,0.));
#15372=DIRECTION('center_axis',(0.,0.,1.));
#15373=DIRECTION('ref_axis',(1.,0.,0.));
#15374=DIRECTION('',(0.,0.,1.));
#15375=DIRECTION('center_axis',(0.,0.,-1.));
#15376=DIRECTION('ref_axis',(1.,0.,0.));
#15377=DIRECTION('center_axis',(0.,0.,1.));
#15378=DIRECTION('ref_axis',(1.,0.,0.));
#15379=DIRECTION('',(0.,0.,1.));
#15380=DIRECTION('center_axis',(0.,0.,-1.));
#15381=DIRECTION('ref_axis',(1.,0.,0.));
#15382=DIRECTION('center_axis',(0.,0.,1.));
#15383=DIRECTION('ref_axis',(1.,0.,0.));
#15384=DIRECTION('center_axis',(0.,0.,1.));
#15385=DIRECTION('ref_axis',(1.,0.,0.));
#15386=DIRECTION('',(0.,0.,1.));
#15387=DIRECTION('center_axis',(0.,0.,-1.));
#15388=DIRECTION('ref_axis',(1.,0.,0.));
#15389=DIRECTION('center_axis',(0.,0.,1.));
#15390=DIRECTION('ref_axis',(1.,0.,0.));
#15391=DIRECTION('center_axis',(0.,0.,1.));
#15392=DIRECTION('ref_axis',(1.,0.,0.));
#15393=DIRECTION('',(0.,0.,1.));
#15394=DIRECTION('center_axis',(0.,0.,-1.));
#15395=DIRECTION('ref_axis',(1.,0.,0.));
#15396=DIRECTION('center_axis',(0.,0.,1.));
#15397=DIRECTION('ref_axis',(1.,0.,0.));
#15398=DIRECTION('center_axis',(0.,0.,1.));
#15399=DIRECTION('ref_axis',(1.,0.,0.));
#15400=DIRECTION('',(0.,0.,1.));
#15401=DIRECTION('center_axis',(0.,0.,-1.));
#15402=DIRECTION('ref_axis',(1.,0.,0.));
#15403=DIRECTION('center_axis',(0.,0.,1.));
#15404=DIRECTION('ref_axis',(1.,0.,0.));
#15405=DIRECTION('center_axis',(0.,0.,1.));
#15406=DIRECTION('ref_axis',(1.,0.,0.));
#15407=DIRECTION('',(0.,0.,1.));
#15408=DIRECTION('center_axis',(0.,0.,-1.));
#15409=DIRECTION('ref_axis',(1.,0.,0.));
#15410=DIRECTION('center_axis',(0.,1.,0.));
#15411=DIRECTION('ref_axis',(-1.,0.,0.));
#15412=DIRECTION('',(-1.,0.,0.));
#15413=DIRECTION('',(0.,0.,1.));
#15414=DIRECTION('',(-1.,0.,0.));
#15415=DIRECTION('',(0.,0.,1.));
#15416=DIRECTION('center_axis',(1.,0.,0.));
#15417=DIRECTION('ref_axis',(0.,1.,0.));
#15418=DIRECTION('',(0.,1.,0.));
#15419=DIRECTION('',(0.,1.,0.));
#15420=DIRECTION('',(0.,0.,1.));
#15421=DIRECTION('center_axis',(0.,-1.,0.));
#15422=DIRECTION('ref_axis',(1.,0.,0.));
#15423=DIRECTION('',(1.,0.,0.));
#15424=DIRECTION('',(1.,0.,0.));
#15425=DIRECTION('',(0.,0.,1.));
#15426=DIRECTION('center_axis',(-1.,0.,0.));
#15427=DIRECTION('ref_axis',(0.,-1.,0.));
#15428=DIRECTION('',(0.,-1.,0.));
#15429=DIRECTION('',(0.,-1.,0.));
#15430=DIRECTION('center_axis',(0.,0.,1.));
#15431=DIRECTION('ref_axis',(1.,0.,0.));
#15432=DIRECTION('center_axis',(0.,0.,1.));
#15433=DIRECTION('ref_axis',(1.,0.,0.));
#15434=DIRECTION('axis',(0.,0.,1.));
#15435=DIRECTION('refdir',(1.,0.,0.));
#15436=DIRECTION('center_axis',(0.,0.,1.));
#15437=DIRECTION('ref_axis',(1.,0.,0.));
#15438=DIRECTION('center_axis',(0.,0.,1.));
#15439=DIRECTION('ref_axis',(1.,0.,0.));
#15440=DIRECTION('',(0.,0.,1.));
#15441=DIRECTION('center_axis',(0.,0.,1.));
#15442=DIRECTION('ref_axis',(1.,0.,0.));
#15443=DIRECTION('center_axis',(0.,0.,1.));
#15444=DIRECTION('ref_axis',(1.,0.,0.));
#15445=DIRECTION('center_axis',(0.,0.,1.));
#15446=DIRECTION('ref_axis',(1.,0.,0.));
#15447=DIRECTION('center_axis',(0.,0.,1.));
#15448=DIRECTION('ref_axis',(1.,0.,0.));
#15449=DIRECTION('',(0.,0.,1.));
#15450=DIRECTION('center_axis',(0.,0.,1.));
#15451=DIRECTION('ref_axis',(1.,0.,0.));
#15452=DIRECTION('center_axis',(0.,0.,1.));
#15453=DIRECTION('ref_axis',(1.,0.,0.));
#15454=DIRECTION('center_axis',(0.,0.,1.));
#15455=DIRECTION('ref_axis',(1.,0.,0.));
#15456=DIRECTION('',(-1.,0.,0.));
#15457=DIRECTION('center_axis',(0.,0.,1.));
#15458=DIRECTION('ref_axis',(1.,0.,0.));
#15459=DIRECTION('',(1.,0.,0.));
#15460=DIRECTION('',(0.,-1.,0.));
#15461=DIRECTION('center_axis',(0.,0.,1.));
#15462=DIRECTION('ref_axis',(1.,0.,0.));
#15463=DIRECTION('',(0.,0.,1.));
#15464=DIRECTION('center_axis',(0.,0.,1.));
#15465=DIRECTION('ref_axis',(1.,0.,0.));
#15466=DIRECTION('',(0.,0.,-1.));
#15467=DIRECTION('center_axis',(0.,0.,1.));
#15468=DIRECTION('ref_axis',(-0.973493764886257,0.228713553878167,0.));
#15469=DIRECTION('',(0.,0.,-1.));
#15470=DIRECTION('center_axis',(0.,0.,1.));
#15471=DIRECTION('ref_axis',(1.,0.,0.));
#15472=DIRECTION('',(0.,0.,1.));
#15473=DIRECTION('center_axis',(0.,0.,1.));
#15474=DIRECTION('ref_axis',(1.,0.,0.));
#15475=DIRECTION('center_axis',(0.,0.,1.));
#15476=DIRECTION('ref_axis',(1.,0.,0.));
#15477=DIRECTION('',(-1.,0.,0.));
#15478=DIRECTION('',(0.,1.,0.));
#15479=DIRECTION('',(1.,0.,0.));
#15480=DIRECTION('center_axis',(-1.,0.,0.));
#15481=DIRECTION('ref_axis',(0.,-1.,0.));
#15482=DIRECTION('',(0.,0.,1.));
#15483=DIRECTION('',(0.,-1.,0.));
#15484=DIRECTION('',(0.,0.,1.));
#15485=DIRECTION('',(0.,-1.,0.));
#15486=DIRECTION('',(0.,0.,1.));
#15487=DIRECTION('center_axis',(0.,-1.,0.));
#15488=DIRECTION('ref_axis',(1.,0.,0.));
#15489=DIRECTION('',(1.,0.,0.));
#15490=DIRECTION('',(0.,0.,1.));
#15491=DIRECTION('',(1.,0.,0.));
#15492=DIRECTION('center_axis',(0.,0.,1.));
#15493=DIRECTION('ref_axis',(1.,0.,0.));
#15494=DIRECTION('center_axis',(0.,0.,1.));
#15495=DIRECTION('ref_axis',(1.,0.,0.));
#15496=DIRECTION('',(0.,0.,1.));
#15497=DIRECTION('center_axis',(0.,0.,-1.));
#15498=DIRECTION('ref_axis',(1.,0.,0.));
#15499=DIRECTION('center_axis',(0.,0.,1.));
#15500=DIRECTION('ref_axis',(1.,0.,0.));
#15501=DIRECTION('center_axis',(0.,0.,1.));
#15502=DIRECTION('ref_axis',(1.,0.,0.));
#15503=DIRECTION('center_axis',(0.,0.,1.));
#15504=DIRECTION('ref_axis',(1.,0.,0.));
#15505=DIRECTION('',(0.,0.,1.));
#15506=DIRECTION('center_axis',(0.,0.,-1.));
#15507=DIRECTION('ref_axis',(1.,0.,0.));
#15508=DIRECTION('center_axis',(0.,0.,1.));
#15509=DIRECTION('ref_axis',(1.,0.,0.));
#15510=DIRECTION('center_axis',(0.,0.,1.));
#15511=DIRECTION('ref_axis',(1.,0.,0.));
#15512=DIRECTION('',(1.,0.,0.));
#15513=DIRECTION('',(0.,1.,0.));
#15514=DIRECTION('',(-1.,0.,0.));
#15515=DIRECTION('center_axis',(0.,-1.,0.));
#15516=DIRECTION('ref_axis',(1.,0.,0.));
#15517=DIRECTION('',(1.,0.,0.));
#15518=DIRECTION('',(0.,0.,1.));
#15519=DIRECTION('center_axis',(0.,0.,1.));
#15520=DIRECTION('ref_axis',(1.,0.,0.));
#15521=DIRECTION('',(0.,1.,0.));
#15522=DIRECTION('center_axis',(0.,1.,0.));
#15523=DIRECTION('ref_axis',(-1.,0.,0.));
#15524=DIRECTION('',(0.,0.,1.));
#15525=DIRECTION('',(-1.,0.,0.));
#15526=DIRECTION('center_axis',(1.,0.,0.));
#15527=DIRECTION('ref_axis',(0.,1.,0.));
#15528=DIRECTION('center_axis',(0.,0.,1.));
#15529=DIRECTION('ref_axis',(1.,0.,0.));
#15530=DIRECTION('axis',(0.,0.,1.));
#15531=DIRECTION('refdir',(1.,0.,0.));
#15532=DIRECTION('center_axis',(0.,1.,0.));
#15533=DIRECTION('ref_axis',(-1.,0.,0.));
#15534=DIRECTION('',(-1.,0.,0.));
#15535=DIRECTION('',(0.,0.,1.));
#15536=DIRECTION('',(-1.,0.,0.));
#15537=DIRECTION('',(0.,0.,1.));
#15538=DIRECTION('center_axis',(1.,0.,0.));
#15539=DIRECTION('ref_axis',(0.,1.,0.));
#15540=DIRECTION('',(0.,1.,0.));
#15541=DIRECTION('',(0.,1.,0.));
#15542=DIRECTION('',(0.,0.,1.));
#15543=DIRECTION('center_axis',(0.,-1.,0.));
#15544=DIRECTION('ref_axis',(1.,0.,0.));
#15545=DIRECTION('',(1.,0.,0.));
#15546=DIRECTION('',(1.,0.,0.));
#15547=DIRECTION('',(0.,0.,1.));
#15548=DIRECTION('center_axis',(-1.,0.,0.));
#15549=DIRECTION('ref_axis',(0.,-1.,0.));
#15550=DIRECTION('',(0.,-1.,0.));
#15551=DIRECTION('',(0.,-1.,0.));
#15552=DIRECTION('center_axis',(0.,0.,1.));
#15553=DIRECTION('ref_axis',(1.,0.,0.));
#15554=DIRECTION('center_axis',(0.,0.,1.));
#15555=DIRECTION('ref_axis',(1.,0.,0.));
#15556=DIRECTION('axis',(0.,0.,1.));
#15557=DIRECTION('refdir',(1.,0.,0.));
#15558=DIRECTION('axis',(0.,0.,1.));
#15559=DIRECTION('refdir',(1.,0.,0.));
#15560=DIRECTION('center_axis',(0.,0.,1.));
#15561=DIRECTION('ref_axis',(1.,0.,0.));
#15562=DIRECTION('',(-1.,0.,0.));
#15563=DIRECTION('center_axis',(0.,0.,1.));
#15564=DIRECTION('ref_axis',(1.,0.,0.));
#15565=DIRECTION('center_axis',(0.,0.,1.));
#15566=DIRECTION('ref_axis',(1.,0.,0.));
#15567=DIRECTION('',(0.,0.,-1.));
#15568=DIRECTION('center_axis',(0.,0.,1.));
#15569=DIRECTION('ref_axis',(1.,0.,0.));
#15570=DIRECTION('',(0.,0.,1.));
#15571=DIRECTION('center_axis',(0.,0.,-1.));
#15572=DIRECTION('ref_axis',(1.,0.,0.));
#15573=DIRECTION('center_axis',(0.,0.,1.));
#15574=DIRECTION('ref_axis',(1.,0.,0.));
#15575=DIRECTION('',(0.,0.,1.));
#15576=DIRECTION('center_axis',(0.,0.,1.));
#15577=DIRECTION('ref_axis',(1.,0.,0.));
#15578=DIRECTION('',(1.,0.,0.));
#15579=DIRECTION('center_axis',(0.,0.,1.));
#15580=DIRECTION('ref_axis',(1.,0.,0.));
#15581=DIRECTION('center_axis',(0.,0.,1.));
#15582=DIRECTION('ref_axis',(1.,0.,0.));
#15583=DIRECTION('',(0.,0.,-1.));
#15584=DIRECTION('center_axis',(0.,0.,1.));
#15585=DIRECTION('ref_axis',(1.,0.,0.));
#15586=DIRECTION('',(0.,0.,1.));
#15587=DIRECTION('center_axis',(0.,0.,-1.));
#15588=DIRECTION('ref_axis',(1.,0.,0.));
#15589=DIRECTION('center_axis',(0.,0.,1.));
#15590=DIRECTION('ref_axis',(1.,0.,0.));
#15591=DIRECTION('',(0.,0.,1.));
#15592=DIRECTION('center_axis',(0.,0.,1.));
#15593=DIRECTION('ref_axis',(1.,0.,0.));
#15594=DIRECTION('',(-1.,0.,0.));
#15595=DIRECTION('center_axis',(0.,0.,1.));
#15596=DIRECTION('ref_axis',(1.,0.,0.));
#15597=DIRECTION('center_axis',(0.,0.,1.));
#15598=DIRECTION('ref_axis',(1.,0.,0.));
#15599=DIRECTION('',(0.,0.,-1.));
#15600=DIRECTION('center_axis',(0.,0.,1.));
#15601=DIRECTION('ref_axis',(1.,0.,0.));
#15602=DIRECTION('',(0.,0.,1.));
#15603=DIRECTION('center_axis',(0.,0.,-1.));
#15604=DIRECTION('ref_axis',(1.,0.,0.));
#15605=DIRECTION('center_axis',(0.,0.,1.));
#15606=DIRECTION('ref_axis',(1.,0.,0.));
#15607=DIRECTION('',(0.,0.,1.));
#15608=DIRECTION('center_axis',(0.,0.,1.));
#15609=DIRECTION('ref_axis',(1.,0.,0.));
#15610=DIRECTION('',(1.,0.,0.));
#15611=DIRECTION('center_axis',(0.,0.,1.));
#15612=DIRECTION('ref_axis',(1.,0.,0.));
#15613=DIRECTION('center_axis',(0.,0.,1.));
#15614=DIRECTION('ref_axis',(1.,0.,0.));
#15615=DIRECTION('',(0.,0.,-1.));
#15616=DIRECTION('center_axis',(0.,0.,1.));
#15617=DIRECTION('ref_axis',(1.,0.,0.));
#15618=DIRECTION('',(0.,0.,1.));
#15619=DIRECTION('center_axis',(0.,0.,-1.));
#15620=DIRECTION('ref_axis',(1.,0.,0.));
#15621=DIRECTION('center_axis',(0.,0.,1.));
#15622=DIRECTION('ref_axis',(1.,0.,0.));
#15623=DIRECTION('',(0.,0.,1.));
#15624=DIRECTION('center_axis',(0.,-1.,0.));
#15625=DIRECTION('ref_axis',(0.,0.,-1.));
#15626=DIRECTION('',(-1.,0.,0.));
#15627=DIRECTION('',(-1.,0.,0.));
#15628=DIRECTION('',(0.,0.,1.));
#15629=DIRECTION('',(1.,0.,0.));
#15630=DIRECTION('',(0.,0.,-1.));
#15631=DIRECTION('',(-1.,0.,0.));
#15632=DIRECTION('center_axis',(0.,1.,0.));
#15633=DIRECTION('ref_axis',(0.,0.,1.));
#15634=DIRECTION('',(1.,0.,0.));
#15635=DIRECTION('',(1.,0.,0.));
#15636=DIRECTION('',(0.,0.,1.));
#15637=DIRECTION('',(1.,0.,0.));
#15638=DIRECTION('',(0.,0.,-1.));
#15639=DIRECTION('',(1.,0.,0.));
#15640=DIRECTION('center_axis',(-1.,0.,0.));
#15641=DIRECTION('ref_axis',(0.,0.,1.));
#15642=DIRECTION('',(0.,-1.,0.));
#15643=DIRECTION('',(0.,0.,1.));
#15644=DIRECTION('',(0.,1.,0.));
#15645=DIRECTION('',(0.,0.,-1.));
#15646=DIRECTION('',(0.,-1.,0.));
#15647=DIRECTION('',(0.,-1.,0.));
#15648=DIRECTION('',(0.,0.,1.));
#15649=DIRECTION('',(0.,-1.,0.));
#15650=DIRECTION('',(0.,0.,-1.));
#15651=DIRECTION('',(0.,-1.,0.));
#15652=DIRECTION('center_axis',(0.,0.,-1.));
#15653=DIRECTION('ref_axis',(0.,1.,0.));
#15654=DIRECTION('',(0.,1.,0.));
#15655=DIRECTION('',(1.,0.,0.));
#15656=DIRECTION('center_axis',(0.,-1.,0.));
#15657=DIRECTION('ref_axis',(0.,0.,-1.));
#15658=DIRECTION('',(0.,0.,-1.));
#15659=DIRECTION('',(1.,0.,0.));
#15660=DIRECTION('center_axis',(0.,0.,1.));
#15661=DIRECTION('ref_axis',(0.,-1.,0.));
#15662=DIRECTION('',(0.,-1.,0.));
#15663=DIRECTION('',(1.,0.,0.));
#15664=DIRECTION('center_axis',(0.,1.,0.));
#15665=DIRECTION('ref_axis',(0.,0.,1.));
#15666=DIRECTION('',(0.,0.,1.));
#15667=DIRECTION('',(1.,0.,0.));
#15668=DIRECTION('center_axis',(0.,0.,-1.));
#15669=DIRECTION('ref_axis',(0.,1.,0.));
#15670=DIRECTION('',(0.,1.,0.));
#15671=DIRECTION('center_axis',(0.,0.,-1.));
#15672=DIRECTION('ref_axis',(0.,1.,0.));
#15673=DIRECTION('',(0.,1.,0.));
#15674=DIRECTION('',(1.,0.,0.));
#15675=DIRECTION('center_axis',(0.,-1.,0.));
#15676=DIRECTION('ref_axis',(0.,0.,-1.));
#15677=DIRECTION('',(0.,0.,-1.));
#15678=DIRECTION('',(1.,0.,0.));
#15679=DIRECTION('center_axis',(0.,0.,-1.));
#15680=DIRECTION('ref_axis',(0.,1.,0.));
#15681=DIRECTION('',(0.,1.,0.));
#15682=DIRECTION('',(1.,0.,0.));
#15683=DIRECTION('center_axis',(0.,1.,0.));
#15684=DIRECTION('ref_axis',(0.,0.,1.));
#15685=DIRECTION('',(0.,0.,1.));
#15686=DIRECTION('',(1.,0.,0.));
#15687=DIRECTION('center_axis',(0.,0.,-1.));
#15688=DIRECTION('ref_axis',(0.,1.,0.));
#15689=DIRECTION('',(0.,1.,0.));
#15690=DIRECTION('center_axis',(1.,0.,0.));
#15691=DIRECTION('ref_axis',(0.,0.,-1.));
#15692=DIRECTION('axis',(0.,0.,1.));
#15693=DIRECTION('refdir',(1.,0.,0.));
#15694=DIRECTION('center_axis',(0.,0.,1.));
#15695=DIRECTION('ref_axis',(0.,-1.,0.));
#15696=DIRECTION('',(0.,-1.,0.));
#15697=DIRECTION('',(1.,0.,0.));
#15698=DIRECTION('',(0.,-1.,0.));
#15699=DIRECTION('',(1.,0.,0.));
#15700=DIRECTION('center_axis',(0.,1.,0.));
#15701=DIRECTION('ref_axis',(0.,0.,1.));
#15702=DIRECTION('',(0.,0.,1.));
#15703=DIRECTION('',(0.,0.,1.));
#15704=DIRECTION('',(1.,0.,0.));
#15705=DIRECTION('center_axis',(0.,0.,-1.));
#15706=DIRECTION('ref_axis',(0.,1.,0.));
#15707=DIRECTION('',(0.,1.,0.));
#15708=DIRECTION('',(0.,1.,0.));
#15709=DIRECTION('',(1.,0.,0.));
#15710=DIRECTION('center_axis',(0.,-1.,0.));
#15711=DIRECTION('ref_axis',(0.,0.,-1.));
#15712=DIRECTION('',(0.,0.,-1.));
#15713=DIRECTION('',(0.,0.,-1.));
#15714=DIRECTION('',(1.,0.,0.));
#15715=DIRECTION('center_axis',(0.,0.,-1.));
#15716=DIRECTION('ref_axis',(0.,1.,0.));
#15717=DIRECTION('',(0.,1.,0.));
#15718=DIRECTION('',(0.,1.,0.));
#15719=DIRECTION('',(1.,0.,0.));
#15720=DIRECTION('center_axis',(0.,1.,0.));
#15721=DIRECTION('ref_axis',(0.,0.,1.));
#15722=DIRECTION('',(0.,0.,1.));
#15723=DIRECTION('',(0.,0.,1.));
#15724=DIRECTION('',(1.,0.,0.));
#15725=DIRECTION('center_axis',(0.,0.,-1.));
#15726=DIRECTION('ref_axis',(0.,1.,0.));
#15727=DIRECTION('',(0.,1.,0.));
#15728=DIRECTION('',(0.,1.,0.));
#15729=DIRECTION('',(1.,0.,0.));
#15730=DIRECTION('center_axis',(0.,-1.,0.));
#15731=DIRECTION('ref_axis',(0.,0.,-1.));
#15732=DIRECTION('',(0.,0.,-1.));
#15733=DIRECTION('',(0.,0.,-1.));
#15734=DIRECTION('center_axis',(1.,0.,0.));
#15735=DIRECTION('ref_axis',(0.,0.,-1.));
#15736=DIRECTION('center_axis',(1.,0.,0.));
#15737=DIRECTION('ref_axis',(0.,0.,-1.));
#15738=DIRECTION('axis',(0.,0.,1.));
#15739=DIRECTION('refdir',(1.,0.,0.));
#15740=DIRECTION('center_axis',(0.,0.,-1.));
#15741=DIRECTION('ref_axis',(0.,-1.,0.));
#15742=DIRECTION('',(0.,1.,0.));
#15743=DIRECTION('',(-1.,0.,0.));
#15744=DIRECTION('',(0.,-1.,0.));
#15745=DIRECTION('',(-1.,0.,0.));
#15746=DIRECTION('center_axis',(0.,1.,0.));
#15747=DIRECTION('ref_axis',(0.,0.,-1.));
#15748=DIRECTION('',(0.,0.,1.));
#15749=DIRECTION('',(0.,0.,-1.));
#15750=DIRECTION('',(-1.,0.,0.));
#15751=DIRECTION('center_axis',(0.,0.,-1.));
#15752=DIRECTION('ref_axis',(0.,-1.,0.));
#15753=DIRECTION('',(0.,1.,0.));
#15754=DIRECTION('',(0.,-1.,0.));
#15755=DIRECTION('',(-1.,0.,0.));
#15756=DIRECTION('center_axis',(0.,-1.,0.));
#15757=DIRECTION('ref_axis',(0.,0.,1.));
#15758=DIRECTION('',(0.,0.,-1.));
#15759=DIRECTION('',(0.,0.,1.));
#15760=DIRECTION('',(-1.,0.,0.));
#15761=DIRECTION('center_axis',(0.,0.,-1.));
#15762=DIRECTION('ref_axis',(0.,-1.,0.));
#15763=DIRECTION('',(0.,1.,0.));
#15764=DIRECTION('',(0.,-1.,0.));
#15765=DIRECTION('',(-1.,0.,0.));
#15766=DIRECTION('center_axis',(0.,1.,0.));
#15767=DIRECTION('ref_axis',(0.,0.,-1.));
#15768=DIRECTION('',(0.,0.,1.));
#15769=DIRECTION('',(0.,0.,-1.));
#15770=DIRECTION('',(-1.,0.,0.));
#15771=DIRECTION('center_axis',(0.,0.,1.));
#15772=DIRECTION('ref_axis',(0.,1.,0.));
#15773=DIRECTION('',(0.,-1.,0.));
#15774=DIRECTION('',(0.,1.,0.));
#15775=DIRECTION('',(-1.,0.,0.));
#15776=DIRECTION('center_axis',(0.,-1.,0.));
#15777=DIRECTION('ref_axis',(0.,0.,1.));
#15778=DIRECTION('',(0.,0.,-1.));
#15779=DIRECTION('',(0.,0.,1.));
#15780=DIRECTION('center_axis',(1.,0.,0.));
#15781=DIRECTION('ref_axis',(0.,0.,-1.));
#15782=DIRECTION('center_axis',(-1.,0.,0.));
#15783=DIRECTION('ref_axis',(0.,0.,1.));
#15784=DIRECTION('',(0.,0.,1.));
#15785=DIRECTION('',(1.,0.,0.));
#15786=DIRECTION('',(0.,0.,1.));
#15787=DIRECTION('',(1.,0.,0.));
#15788=DIRECTION('',(0.,0.,1.));
#15789=DIRECTION('',(1.,0.,0.));
#15790=DIRECTION('axis',(0.,0.,1.));
#15791=DIRECTION('refdir',(1.,0.,0.));
#15792=DIRECTION('center_axis',(0.,1.,0.));
#15793=DIRECTION('ref_axis',(1.,0.,0.));
#15794=DIRECTION('center_axis',(0.,1.,0.));
#15795=DIRECTION('ref_axis',(1.,0.,0.));
#15796=DIRECTION('',(0.707106781186548,-0.707106781186547,-8.65956056235494E-17));
#15797=DIRECTION('center_axis',(0.,-1.,0.));
#15798=DIRECTION('ref_axis',(1.,0.,0.));
#15799=DIRECTION('center_axis',(0.,1.,0.));
#15800=DIRECTION('ref_axis',(1.,0.,0.));
#15801=DIRECTION('',(0.,-1.,0.));
#15802=DIRECTION('center_axis',(0.,-1.,0.));
#15803=DIRECTION('ref_axis',(1.,0.,0.));
#15804=DIRECTION('center_axis',(0.,1.,0.));
#15805=DIRECTION('ref_axis',(1.,0.,0.));
#15806=DIRECTION('center_axis',(0.,1.,0.));
#15807=DIRECTION('ref_axis',(1.,0.,0.));
#15808=DIRECTION('center_axis',(0.,1.,0.));
#15809=DIRECTION('ref_axis',(1.,0.,0.));
#15810=DIRECTION('',(0.,-1.,0.));
#15811=DIRECTION('center_axis',(0.,1.,0.));
#15812=DIRECTION('ref_axis',(1.,0.,0.));
#15813=DIRECTION('center_axis',(0.,1.,0.));
#15814=DIRECTION('ref_axis',(1.,0.,0.));
#15815=DIRECTION('axis',(0.,0.,1.));
#15816=DIRECTION('refdir',(1.,0.,0.));
#15817=DIRECTION('center_axis',(0.,1.,0.));
#15818=DIRECTION('ref_axis',(0.,0.,1.));
#15819=DIRECTION('center_axis',(0.,-1.,0.));
#15820=DIRECTION('ref_axis',(1.,0.,0.));
#15821=DIRECTION('center_axis',(0.,-1.,0.));
#15822=DIRECTION('ref_axis',(1.,0.,0.));
#15823=DIRECTION('center_axis',(0.,-1.,0.));
#15824=DIRECTION('ref_axis',(1.,0.,0.));
#15825=DIRECTION('',(0.707106781186548,0.707106781186547,8.65956056235493E-17));
#15826=DIRECTION('center_axis',(0.,-1.,0.));
#15827=DIRECTION('ref_axis',(1.,0.,0.));
#15828=DIRECTION('center_axis',(0.,-1.,0.));
#15829=DIRECTION('ref_axis',(1.,0.,0.));
#15830=DIRECTION('',(0.,1.,0.));
#15831=DIRECTION('center_axis',(0.,1.,0.));
#15832=DIRECTION('ref_axis',(1.,0.,0.));
#15833=DIRECTION('center_axis',(0.,-1.,0.));
#15834=DIRECTION('ref_axis',(1.,0.,0.));
#15835=DIRECTION('',(-0.707106781186547,0.707106781186548,-8.65956056235493E-17));
#15836=DIRECTION('center_axis',(0.,-1.,0.));
#15837=DIRECTION('ref_axis',(0.,0.,-1.));
#15838=DIRECTION('center_axis',(0.,-1.,0.));
#15839=DIRECTION('ref_axis',(1.,0.,0.));
#15840=DIRECTION('center_axis',(0.,1.,0.));
#15841=DIRECTION('ref_axis',(1.,0.,0.));
#15842=DIRECTION('center_axis',(0.,1.,0.));
#15843=DIRECTION('ref_axis',(1.,0.,0.));
#15844=DIRECTION('',(-0.447213595499958,0.894427190999916,-5.47678698264203E-17));
#15845=DIRECTION('center_axis',(0.,-1.,0.));
#15846=DIRECTION('ref_axis',(1.,0.,0.));
#15847=DIRECTION('center_axis',(0.,1.,0.));
#15848=DIRECTION('ref_axis',(1.,0.,0.));
#15849=DIRECTION('',(0.,1.,0.));
#15850=DIRECTION('center_axis',(0.,1.,0.));
#15851=DIRECTION('ref_axis',(1.,0.,0.));
#15852=DIRECTION('center_axis',(0.,-1.,0.));
#15853=DIRECTION('ref_axis',(1.,0.,0.));
#15854=DIRECTION('',(-0.707106781186547,0.707106781186548,-8.65956056235493E-17));
#15855=DIRECTION('center_axis',(0.,-1.,0.));
#15856=DIRECTION('ref_axis',(0.,0.,-1.));
#15857=DIRECTION('center_axis',(0.866025403784439,0.,-0.5));
#15858=DIRECTION('ref_axis',(0.5,0.,0.866025403784439));
#15859=DIRECTION('',(-0.5,0.,-0.866025403784439));
#15860=DIRECTION('',(0.,-1.,0.));
#15861=DIRECTION('',(0.5,0.,0.866025403784439));
#15862=DIRECTION('',(0.,-1.,0.));
#15863=DIRECTION('center_axis',(1.20185167898973E-16,0.,-1.));
#15864=DIRECTION('ref_axis',(1.,0.,1.20185167898973E-16));
#15865=DIRECTION('',(-1.,0.,-1.20185167898973E-16));
#15866=DIRECTION('',(0.,-1.,0.));
#15867=DIRECTION('',(1.,0.,1.20185167898973E-16));
#15868=DIRECTION('center_axis',(-0.866025403784439,0.,-0.5));
#15869=DIRECTION('ref_axis',(0.5,0.,-0.866025403784439));
#15870=DIRECTION('',(-0.5,0.,0.866025403784439));
#15871=DIRECTION('',(0.,-1.,0.));
#15872=DIRECTION('',(0.5,0.,-0.866025403784439));
#15873=DIRECTION('center_axis',(-0.866025403784439,0.,0.5));
#15874=DIRECTION('ref_axis',(-0.5,0.,-0.866025403784439));
#15875=DIRECTION('',(0.5,0.,0.866025403784439));
#15876=DIRECTION('',(0.,-1.,0.));
#15877=DIRECTION('',(-0.5,0.,-0.866025403784439));
#15878=DIRECTION('center_axis',(-2.40370335797945E-16,0.,1.));
#15879=DIRECTION('ref_axis',(-1.,0.,-2.40370335797945E-16));
#15880=DIRECTION('',(1.,0.,2.40370335797945E-16));
#15881=DIRECTION('',(0.,-1.,0.));
#15882=DIRECTION('',(-1.,0.,-2.40370335797945E-16));
#15883=DIRECTION('center_axis',(0.866025403784439,0.,0.5));
#15884=DIRECTION('ref_axis',(-0.5,0.,0.866025403784439));
#15885=DIRECTION('',(0.5,0.,-0.866025403784439));
#15886=DIRECTION('',(-0.5,0.,0.866025403784439));
#15887=DIRECTION('center_axis',(0.,1.,0.));
#15888=DIRECTION('ref_axis',(1.,0.,0.));
#15889=DIRECTION('center_axis',(0.,-1.,0.));
#15890=DIRECTION('ref_axis',(0.,0.,-1.));
#15891=DIRECTION('axis',(0.,0.,1.));
#15892=DIRECTION('refdir',(1.,0.,0.));
#15893=DIRECTION('center_axis',(0.866025403784439,0.,-0.5));
#15894=DIRECTION('ref_axis',(0.5,0.,0.866025403784439));
#15895=DIRECTION('',(-0.5,0.,-0.866025403784439));
#15896=DIRECTION('',(0.,-1.,0.));
#15897=DIRECTION('',(0.5,0.,0.866025403784439));
#15898=DIRECTION('',(0.,-1.,0.));
#15899=DIRECTION('center_axis',(1.60246890531964E-16,0.,-1.));
#15900=DIRECTION('ref_axis',(1.,0.,1.60246890531964E-16));
#15901=DIRECTION('',(-1.,0.,-1.60246890531964E-16));
#15902=DIRECTION('',(0.,-1.,0.));
#15903=DIRECTION('',(1.,0.,1.60246890531964E-16));
#15904=DIRECTION('center_axis',(-0.866025403784439,0.,-0.5));
#15905=DIRECTION('ref_axis',(0.5,0.,-0.866025403784439));
#15906=DIRECTION('',(-0.5,0.,0.866025403784439));
#15907=DIRECTION('',(0.,-1.,0.));
#15908=DIRECTION('',(0.5,0.,-0.866025403784439));
#15909=DIRECTION('center_axis',(-0.866025403784439,0.,0.5));
#15910=DIRECTION('ref_axis',(-0.5,0.,-0.866025403784439));
#15911=DIRECTION('',(0.5,0.,0.866025403784439));
#15912=DIRECTION('',(0.,-1.,0.));
#15913=DIRECTION('',(-0.5,0.,-0.866025403784439));
#15914=DIRECTION('center_axis',(-1.60246890531964E-16,0.,1.));
#15915=DIRECTION('ref_axis',(-1.,0.,-1.60246890531964E-16));
#15916=DIRECTION('',(1.,0.,1.60246890531964E-16));
#15917=DIRECTION('',(0.,-1.,0.));
#15918=DIRECTION('',(-1.,0.,-1.60246890531964E-16));
#15919=DIRECTION('center_axis',(0.866025403784439,0.,0.5));
#15920=DIRECTION('ref_axis',(-0.5,0.,0.866025403784439));
#15921=DIRECTION('',(0.5,0.,-0.866025403784439));
#15922=DIRECTION('',(-0.5,0.,0.866025403784439));
#15923=DIRECTION('center_axis',(0.,1.,0.));
#15924=DIRECTION('ref_axis',(1.,0.,0.));
#15925=DIRECTION('center_axis',(0.,-1.,0.));
#15926=DIRECTION('ref_axis',(0.,0.,-1.));
#15927=DIRECTION('center_axis',(0.,1.,0.));
#15928=DIRECTION('ref_axis',(1.,0.,0.));
#15929=DIRECTION('center_axis',(0.,1.,0.));
#15930=DIRECTION('ref_axis',(1.,0.,0.));
#15931=DIRECTION('center_axis',(0.,1.,0.));
#15932=DIRECTION('ref_axis',(0.,0.,1.));
#15933=DIRECTION('center_axis',(0.,-1.,0.));
#15934=DIRECTION('ref_axis',(1.,0.,0.));
#15935=DIRECTION('center_axis',(0.,-1.,0.));
#15936=DIRECTION('ref_axis',(1.,0.,0.));
#15937=DIRECTION('center_axis',(0.,-1.,0.));
#15938=DIRECTION('ref_axis',(1.,0.,0.));
#15939=DIRECTION('',(0.707106781186547,0.707106781186548,8.65956056235493E-17));
#15940=DIRECTION('center_axis',(0.,-1.,0.));
#15941=DIRECTION('ref_axis',(1.,0.,0.));
#15942=DIRECTION('center_axis',(0.,-1.,0.));
#15943=DIRECTION('ref_axis',(1.,0.,0.));
#15944=DIRECTION('',(0.,1.,0.));
#15945=DIRECTION('center_axis',(0.,1.,0.));
#15946=DIRECTION('ref_axis',(1.,0.,0.));
#15947=DIRECTION('center_axis',(0.,-1.,0.));
#15948=DIRECTION('ref_axis',(1.,0.,0.));
#15949=DIRECTION('',(-0.707106781186547,0.707106781186548,-8.65956056235493E-17));
#15950=DIRECTION('center_axis',(0.,-1.,0.));
#15951=DIRECTION('ref_axis',(0.,0.,-1.));
#15952=DIRECTION('center_axis',(0.,-1.,0.));
#15953=DIRECTION('ref_axis',(1.,0.,0.));
#15954=DIRECTION('center_axis',(0.,1.,0.));
#15955=DIRECTION('ref_axis',(1.,0.,0.));
#15956=DIRECTION('center_axis',(0.,1.,0.));
#15957=DIRECTION('ref_axis',(1.,0.,0.));
#15958=DIRECTION('',(-0.447213595499958,0.894427190999916,-5.47678698264203E-17));
#15959=DIRECTION('center_axis',(0.,-1.,0.));
#15960=DIRECTION('ref_axis',(1.,0.,0.));
#15961=DIRECTION('',(0.,1.,0.));
#15962=DIRECTION('axis',(0.,0.,1.));
#15963=DIRECTION('refdir',(1.,0.,0.));
#15964=DIRECTION('center_axis',(0.,1.,0.));
#15965=DIRECTION('ref_axis',(0.,0.,1.));
#15966=DIRECTION('center_axis',(0.,-1.,0.));
#15967=DIRECTION('ref_axis',(1.,0.,0.));
#15968=DIRECTION('center_axis',(0.,-1.,0.));
#15969=DIRECTION('ref_axis',(1.,0.,0.));
#15970=DIRECTION('center_axis',(0.,-1.,0.));
#15971=DIRECTION('ref_axis',(1.,0.,0.));
#15972=DIRECTION('',(0.707106781186547,0.707106781186548,8.65956056235493E-17));
#15973=DIRECTION('center_axis',(0.,-1.,0.));
#15974=DIRECTION('ref_axis',(1.,0.,0.));
#15975=DIRECTION('center_axis',(0.,-1.,0.));
#15976=DIRECTION('ref_axis',(1.,0.,0.));
#15977=DIRECTION('',(0.,1.,0.));
#15978=DIRECTION('center_axis',(0.,1.,0.));
#15979=DIRECTION('ref_axis',(1.,0.,0.));
#15980=DIRECTION('center_axis',(0.,-1.,0.));
#15981=DIRECTION('ref_axis',(1.,0.,0.));
#15982=DIRECTION('',(-0.707106781186547,0.707106781186548,-8.65956056235493E-17));
#15983=DIRECTION('center_axis',(0.,-1.,0.));
#15984=DIRECTION('ref_axis',(0.,0.,-1.));
#15985=DIRECTION('center_axis',(0.,-1.,0.));
#15986=DIRECTION('ref_axis',(1.,0.,0.));
#15987=DIRECTION('center_axis',(0.,1.,0.));
#15988=DIRECTION('ref_axis',(1.,0.,0.));
#15989=DIRECTION('center_axis',(0.,1.,0.));
#15990=DIRECTION('ref_axis',(1.,0.,0.));
#15991=DIRECTION('',(-0.447213595499958,0.894427190999916,-5.47678698264203E-17));
#15992=DIRECTION('center_axis',(0.,-1.,0.));
#15993=DIRECTION('ref_axis',(1.,0.,0.));
#15994=DIRECTION('center_axis',(0.,1.,0.));
#15995=DIRECTION('ref_axis',(1.,0.,0.));
#15996=DIRECTION('',(0.,1.,0.));
#15997=DIRECTION('center_axis',(0.,1.,0.));
#15998=DIRECTION('ref_axis',(1.,0.,0.));
#15999=DIRECTION('center_axis',(0.,-1.,0.));
#16000=DIRECTION('ref_axis',(1.,0.,0.));
#16001=DIRECTION('',(-0.707106781186547,0.707106781186548,-8.65956056235493E-17));
#16002=DIRECTION('center_axis',(0.,-1.,0.));
#16003=DIRECTION('ref_axis',(0.,0.,-1.));
#16004=DIRECTION('center_axis',(0.866025403784439,0.,-0.5));
#16005=DIRECTION('ref_axis',(0.5,0.,0.866025403784439));
#16006=DIRECTION('',(-0.5,0.,-0.866025403784439));
#16007=DIRECTION('',(0.,-1.,0.));
#16008=DIRECTION('',(0.5,0.,0.866025403784439));
#16009=DIRECTION('',(0.,-1.,0.));
#16010=DIRECTION('center_axis',(1.60246890531964E-16,0.,-1.));
#16011=DIRECTION('ref_axis',(1.,0.,1.60246890531964E-16));
#16012=DIRECTION('',(-1.,0.,-1.60246890531964E-16));
#16013=DIRECTION('',(0.,-1.,0.));
#16014=DIRECTION('',(1.,0.,1.60246890531964E-16));
#16015=DIRECTION('center_axis',(-0.866025403784439,0.,-0.5));
#16016=DIRECTION('ref_axis',(0.5,0.,-0.866025403784439));
#16017=DIRECTION('',(-0.5,0.,0.866025403784439));
#16018=DIRECTION('',(0.,-1.,0.));
#16019=DIRECTION('',(0.5,0.,-0.866025403784439));
#16020=DIRECTION('center_axis',(-0.866025403784439,0.,0.5));
#16021=DIRECTION('ref_axis',(-0.5,0.,-0.866025403784439));
#16022=DIRECTION('',(0.5,0.,0.866025403784439));
#16023=DIRECTION('',(0.,-1.,0.));
#16024=DIRECTION('',(-0.5,0.,-0.866025403784439));
#16025=DIRECTION('center_axis',(-1.60246890531964E-16,0.,1.));
#16026=DIRECTION('ref_axis',(-1.,0.,-1.60246890531964E-16));
#16027=DIRECTION('',(1.,0.,1.60246890531964E-16));
#16028=DIRECTION('',(0.,-1.,0.));
#16029=DIRECTION('',(-1.,0.,-1.60246890531964E-16));
#16030=DIRECTION('center_axis',(0.866025403784439,0.,0.5));
#16031=DIRECTION('ref_axis',(-0.5,0.,0.866025403784439));
#16032=DIRECTION('',(0.5,0.,-0.866025403784439));
#16033=DIRECTION('',(-0.5,0.,0.866025403784439));
#16034=DIRECTION('center_axis',(0.,1.,0.));
#16035=DIRECTION('ref_axis',(1.,0.,0.));
#16036=DIRECTION('center_axis',(0.,-1.,0.));
#16037=DIRECTION('ref_axis',(0.,0.,-1.));
#16038=DIRECTION('',(0.,0.,1.));
#16039=DIRECTION('',(1.,0.,0.));
#16040=DIRECTION('',(0.,0.,1.));
#16041=DIRECTION('',(1.,0.,0.));
#16042=DIRECTION('',(0.,0.,1.));
#16043=DIRECTION('',(1.,0.,0.));
#16044=DIRECTION('',(0.,0.,1.));
#16045=DIRECTION('',(1.,0.,0.));
#16046=DIRECTION('',(0.,0.,1.));
#16047=DIRECTION('',(1.,0.,0.));
#16048=DIRECTION('',(0.,0.,1.));
#16049=DIRECTION('',(1.,0.,0.));
#16050=DIRECTION('',(0.,0.,1.));
#16051=DIRECTION('',(1.,0.,0.));
#16052=DIRECTION('',(0.,0.,1.));
#16053=DIRECTION('',(1.,0.,0.));
#16054=DIRECTION('',(0.,0.,1.));
#16055=DIRECTION('',(1.,0.,0.));
#16056=DIRECTION('',(0.,0.,1.));
#16057=DIRECTION('',(1.,0.,0.));
#16058=DIRECTION('',(0.,0.,1.));
#16059=DIRECTION('',(1.,0.,0.));
#16060=DIRECTION('',(0.,0.,1.));
#16061=DIRECTION('',(1.,0.,0.));
#16062=DIRECTION('',(0.,0.,1.));
#16063=DIRECTION('',(1.,0.,0.));
#16064=DIRECTION('',(0.,0.,1.));
#16065=DIRECTION('',(1.,0.,0.));
#16066=DIRECTION('',(0.,-1.,2.22044604925031E-16));
#16067=DIRECTION('',(1.,0.,0.));
#16068=DIRECTION('',(0.,-1.,2.22044604925031E-16));
#16069=DIRECTION('',(1.,0.,0.));
#16070=DIRECTION('',(0.,-1.,2.22044604925031E-16));
#16071=DIRECTION('',(1.,0.,0.));
#16072=DIRECTION('',(0.,-1.,2.22044604925031E-16));
#16073=DIRECTION('',(1.,0.,0.));
#16074=DIRECTION('',(0.,0.,1.));
#16075=DIRECTION('',(1.,0.,0.));
#16076=DIRECTION('',(0.,0.,1.));
#16077=DIRECTION('',(1.,0.,0.));
#16078=DIRECTION('',(0.,0.,1.));
#16079=DIRECTION('',(-1.,1.22464679914735E-16,0.));
#16080=DIRECTION('',(0.,0.,1.));
#16081=DIRECTION('',(-1.,1.22464679914735E-16,0.));
#16082=DIRECTION('',(0.,0.,1.));
#16083=DIRECTION('',(-1.,1.22464679914735E-16,0.));
#16084=DIRECTION('',(0.,0.,1.));
#16085=DIRECTION('',(-1.,1.22464679914735E-16,0.));
#16086=DIRECTION('',(0.,0.,1.));
#16087=DIRECTION('',(1.,0.,0.));
#16088=DIRECTION('',(0.,0.,1.));
#16089=DIRECTION('',(1.,0.,0.));
#16090=DIRECTION('',(0.,0.,1.));
#16091=DIRECTION('',(1.,0.,0.));
#16092=DIRECTION('',(0.,0.,1.));
#16093=DIRECTION('',(1.,0.,0.));
#16094=DIRECTION('',(0.,-1.,2.22044604925031E-16));
#16095=DIRECTION('',(1.,0.,0.));
#16096=DIRECTION('',(0.,-1.,2.22044604925031E-16));
#16097=DIRECTION('',(1.,0.,0.));
#16098=DIRECTION('',(0.,-1.,2.22044604925031E-16));
#16099=DIRECTION('',(1.,0.,0.));
#16100=DIRECTION('',(0.,-1.,2.22044604925031E-16));
#16101=DIRECTION('',(1.,0.,0.));
#16102=DIRECTION('',(0.,0.,1.));
#16103=DIRECTION('',(1.,0.,0.));
#16104=DIRECTION('',(0.,0.,1.));
#16105=DIRECTION('',(1.,0.,0.));
#16106=DIRECTION('',(0.,0.,1.));
#16107=DIRECTION('',(-1.,1.22464679914735E-16,0.));
#16108=DIRECTION('',(0.,0.,1.));
#16109=DIRECTION('',(-1.,1.22464679914735E-16,0.));
#16110=DIRECTION('',(0.,0.,1.));
#16111=DIRECTION('',(-1.,1.22464679914735E-16,0.));
#16112=DIRECTION('',(0.,0.,1.));
#16113=DIRECTION('',(-1.,1.22464679914735E-16,0.));
#16114=DIRECTION('',(0.,0.,1.));
#16115=DIRECTION('',(1.,0.,0.));
#16116=DIRECTION('',(0.,0.,1.));
#16117=DIRECTION('',(1.,0.,0.));
#16118=DIRECTION('',(0.,0.,1.));
#16119=DIRECTION('',(1.,0.,0.));
#16120=DIRECTION('',(0.,0.,1.));
#16121=DIRECTION('',(1.,0.,0.));
#16122=DIRECTION('',(0.,0.,1.));
#16123=DIRECTION('',(1.,0.,0.));
#16124=DIRECTION('',(0.,0.,1.));
#16125=DIRECTION('',(1.,0.,0.));
#16126=DIRECTION('',(0.,-1.,2.22044604925031E-16));
#16127=DIRECTION('',(1.,0.,0.));
#16128=DIRECTION('',(0.,0.,1.));
#16129=DIRECTION('',(1.,0.,0.));
#16130=DIRECTION('',(0.,-1.,2.22044604925031E-16));
#16131=DIRECTION('',(1.,0.,0.));
#16132=DIRECTION('',(0.,0.,1.));
#16133=DIRECTION('',(1.,0.,0.));
#16134=DIRECTION('',(0.,0.,1.));
#16135=DIRECTION('',(1.,0.,0.));
#16136=DIRECTION('',(0.,-1.,2.22044604925031E-16));
#16137=DIRECTION('',(1.,0.,0.));
#16138=DIRECTION('',(0.,0.,1.));
#16139=DIRECTION('',(1.,0.,0.));
#16140=DIRECTION('',(0.,-1.,2.22044604925031E-16));
#16141=DIRECTION('',(1.,0.,0.));
#16142=DIRECTION('',(0.,0.,1.));
#16143=DIRECTION('',(1.,0.,0.));
#16144=DIRECTION('',(0.,-1.,2.22044604925031E-16));
#16145=DIRECTION('',(1.,0.,0.));
#16146=DIRECTION('',(0.,-1.,2.22044604925031E-16));
#16147=DIRECTION('',(1.,0.,0.));
#16148=DIRECTION('',(0.,-1.,2.22044604925031E-16));
#16149=DIRECTION('',(1.,0.,0.));
#16150=DIRECTION('',(0.,-1.,2.22044604925031E-16));
#16151=DIRECTION('',(1.,0.,0.));
#16152=DIRECTION('',(0.,-1.,2.22044604925031E-16));
#16153=DIRECTION('',(1.,0.,0.));
#16154=DIRECTION('',(0.,-1.,2.22044604925031E-16));
#16155=DIRECTION('',(1.,0.,0.));
#16156=DIRECTION('',(0.,-1.,2.22044604925031E-16));
#16157=DIRECTION('',(1.,0.,0.));
#16158=DIRECTION('',(0.,-1.,2.22044604925031E-16));
#16159=DIRECTION('',(1.,0.,0.));
#16160=DIRECTION('',(0.,0.,1.));
#16161=DIRECTION('',(1.,0.,0.));
#16162=DIRECTION('',(0.,0.,1.));
#16163=DIRECTION('',(1.,0.,0.));
#16164=DIRECTION('',(0.,0.,1.));
#16165=DIRECTION('',(1.,0.,0.));
#16166=DIRECTION('',(0.,0.,1.));
#16167=DIRECTION('',(1.,0.,0.));
#16168=DIRECTION('',(0.,0.,1.));
#16169=DIRECTION('',(1.,0.,0.));
#16170=DIRECTION('',(0.,0.,1.));
#16171=DIRECTION('',(1.,0.,0.));
#16172=DIRECTION('',(0.,0.,1.));
#16173=DIRECTION('',(1.,0.,0.));
#16174=DIRECTION('',(0.,0.,1.));
#16175=DIRECTION('',(-1.,1.22464679914735E-16,0.));
#16176=DIRECTION('',(0.,0.,1.));
#16177=DIRECTION('',(1.,0.,0.));
#16178=DIRECTION('',(0.,0.,1.));
#16179=DIRECTION('',(1.,0.,0.));
#16180=DIRECTION('',(0.,0.,1.));
#16181=DIRECTION('',(1.,0.,0.));
#16182=DIRECTION('',(0.,0.,1.));
#16183=DIRECTION('',(1.,0.,0.));
#16184=DIRECTION('',(0.,0.,1.));
#16185=DIRECTION('',(1.,0.,0.));
#16186=DIRECTION('',(0.,0.,1.));
#16187=DIRECTION('',(1.,0.,0.));
#16188=DIRECTION('',(0.,0.,1.));
#16189=DIRECTION('',(1.,0.,0.));
#16190=DIRECTION('',(0.,0.,1.));
#16191=DIRECTION('',(-1.,1.22464679914735E-16,0.));
#16192=DIRECTION('',(0.,0.,1.));
#16193=DIRECTION('',(1.,0.,0.));
#16194=DIRECTION('',(0.,0.,1.));
#16195=DIRECTION('',(1.,0.,0.));
#16196=DIRECTION('',(0.,0.,1.));
#16197=DIRECTION('',(1.,0.,0.));
#16198=DIRECTION('',(0.,0.,1.));
#16199=DIRECTION('',(1.,0.,0.));
#16200=DIRECTION('',(0.,-1.,2.22044604925031E-16));
#16201=DIRECTION('',(1.,0.,0.));
#16202=DIRECTION('',(0.,-1.,2.22044604925031E-16));
#16203=DIRECTION('',(1.,0.,0.));
#16204=DIRECTION('',(0.,-1.,2.22044604925031E-16));
#16205=DIRECTION('',(1.,0.,0.));
#16206=DIRECTION('',(0.,-1.,2.22044604925031E-16));
#16207=DIRECTION('',(1.,0.,0.));
#16208=DIRECTION('',(0.,-1.,2.22044604925031E-16));
#16209=DIRECTION('',(1.,0.,0.));
#16210=DIRECTION('',(0.,-1.,2.22044604925031E-16));
#16211=DIRECTION('',(1.,0.,0.));
#16212=DIRECTION('',(0.,-1.,2.22044604925031E-16));
#16213=DIRECTION('',(1.,0.,0.));
#16214=DIRECTION('',(0.,-1.,2.22044604925031E-16));
#16215=DIRECTION('',(1.,0.,0.));
#16216=DIRECTION('',(0.,-1.,2.22044604925031E-16));
#16217=DIRECTION('',(1.,0.,0.));
#16218=DIRECTION('',(0.,-1.,2.22044604925031E-16));
#16219=DIRECTION('',(1.,0.,0.));
#16220=DIRECTION('',(0.,1.,2.22044604925031E-16));
#16221=DIRECTION('',(1.,0.,0.));
#16222=DIRECTION('',(0.,1.,2.22044604925031E-16));
#16223=DIRECTION('',(1.,0.,0.));
#16224=DIRECTION('',(0.,0.,1.));
#16225=DIRECTION('',(1.,0.,0.));
#16226=DIRECTION('',(0.,0.,1.));
#16227=DIRECTION('',(1.,0.,0.));
#16228=DIRECTION('',(0.,0.,1.));
#16229=DIRECTION('',(1.,0.,0.));
#16230=DIRECTION('',(0.,0.,1.));
#16231=DIRECTION('',(1.,0.,0.));
#16232=CARTESIAN_POINT('',(0.,0.,0.));
#16233=CARTESIAN_POINT('',(0.,0.,0.));
#16234=CARTESIAN_POINT('',(0.,0.,0.));
#16235=CARTESIAN_POINT('Origin',(26.2,-2.5,-0.9));
#16236=CARTESIAN_POINT('',(26.035,-2.5,-0.9));
#16237=CARTESIAN_POINT('Origin',(26.2,-2.5,-0.9));
#16238=CARTESIAN_POINT('',(26.035,-2.5,0.));
#16239=CARTESIAN_POINT('',(26.035,-2.5,-0.9));
#16240=CARTESIAN_POINT('Origin',(26.2,-2.5,0.));
#16241=CARTESIAN_POINT('Origin',(26.2,-2.5,-0.9));
#16242=CARTESIAN_POINT('Origin',(26.2,2.5,-0.9));
#16243=CARTESIAN_POINT('',(26.035,2.5,-0.9));
#16244=CARTESIAN_POINT('Origin',(26.2,2.5,-0.9));
#16245=CARTESIAN_POINT('',(26.035,2.5,0.));
#16246=CARTESIAN_POINT('',(26.035,2.5,-0.9));
#16247=CARTESIAN_POINT('Origin',(26.2,2.5,0.));
#16248=CARTESIAN_POINT('Origin',(26.2,2.5,-0.9));
#16249=CARTESIAN_POINT('Origin',(5.8,-2.5,-0.9));
#16250=CARTESIAN_POINT('',(5.635,-2.5,-0.9));
#16251=CARTESIAN_POINT('Origin',(5.8,-2.5,-0.9));
#16252=CARTESIAN_POINT('',(5.635,-2.5,0.));
#16253=CARTESIAN_POINT('',(5.635,-2.5,-0.9));
#16254=CARTESIAN_POINT('Origin',(5.8,-2.5,0.));
#16255=CARTESIAN_POINT('Origin',(5.8,-2.5,-0.9));
#16256=CARTESIAN_POINT('Origin',(5.8,2.5,-0.9));
#16257=CARTESIAN_POINT('',(5.635,2.5,-0.9));
#16258=CARTESIAN_POINT('Origin',(5.8,2.5,-0.9));
#16259=CARTESIAN_POINT('',(5.635,2.5,0.));
#16260=CARTESIAN_POINT('',(5.635,2.5,-0.9));
#16261=CARTESIAN_POINT('Origin',(5.8,2.5,0.));
#16262=CARTESIAN_POINT('Origin',(5.8,2.5,-0.9));
#16263=CARTESIAN_POINT('Origin',(25.,0.,-1.1));
#16264=CARTESIAN_POINT('',(24.835,-2.02066721859312E-17,-1.1));
#16265=CARTESIAN_POINT('Origin',(25.,0.,-1.1));
#16266=CARTESIAN_POINT('',(24.835,2.02066721859312E-17,0.));
#16267=CARTESIAN_POINT('',(24.835,-2.02066721859312E-17,-1.1));
#16268=CARTESIAN_POINT('Origin',(25.,0.,0.));
#16269=CARTESIAN_POINT('Origin',(25.,0.,-1.1));
#16270=CARTESIAN_POINT('Origin',(19.,0.,-1.1));
#16271=CARTESIAN_POINT('',(18.835,-2.02066721859312E-17,-1.1));
#16272=CARTESIAN_POINT('Origin',(19.,0.,-1.1));
#16273=CARTESIAN_POINT('',(18.835,2.02066721859312E-17,0.));
#16274=CARTESIAN_POINT('',(18.835,-2.02066721859312E-17,-1.1));
#16275=CARTESIAN_POINT('Origin',(19.,0.,0.));
#16276=CARTESIAN_POINT('Origin',(19.,0.,-1.1));
#16277=CARTESIAN_POINT('Origin',(13.,0.,-1.1));
#16278=CARTESIAN_POINT('',(12.835,-2.02066721859312E-17,-1.1));
#16279=CARTESIAN_POINT('Origin',(13.,0.,-1.1));
#16280=CARTESIAN_POINT('',(12.835,2.02066721859312E-17,0.));
#16281=CARTESIAN_POINT('',(12.835,-2.02066721859312E-17,-1.1));
#16282=CARTESIAN_POINT('Origin',(13.,0.,0.));
#16283=CARTESIAN_POINT('Origin',(13.,0.,-1.1));
#16284=CARTESIAN_POINT('Origin',(7.,0.,-1.1));
#16285=CARTESIAN_POINT('',(6.835,-2.02066721859313E-17,-1.1));
#16286=CARTESIAN_POINT('Origin',(7.,0.,-1.1));
#16287=CARTESIAN_POINT('',(6.835,2.02066721859313E-17,0.));
#16288=CARTESIAN_POINT('',(6.835,-2.02066721859313E-17,-1.1));
#16289=CARTESIAN_POINT('Origin',(7.,0.,0.));
#16290=CARTESIAN_POINT('Origin',(7.,0.,-1.1));
#16291=CARTESIAN_POINT('Origin',(27.,3.5,-1.3));
#16292=CARTESIAN_POINT('',(26.725,3.5,-1.2));
#16293=CARTESIAN_POINT('Origin',(27.,3.5,-1.2));
#16294=CARTESIAN_POINT('',(26.725,3.5,0.));
#16295=CARTESIAN_POINT('',(26.725,3.5,-1.3));
#16296=CARTESIAN_POINT('Origin',(27.,3.5,0.));
#16297=CARTESIAN_POINT('Origin',(5.,3.5,-1.3));
#16298=CARTESIAN_POINT('',(4.725,3.5,-1.2));
#16299=CARTESIAN_POINT('Origin',(5.,3.5,-1.2));
#16300=CARTESIAN_POINT('',(4.725,3.5,0.));
#16301=CARTESIAN_POINT('',(4.725,3.5,-1.3));
#16302=CARTESIAN_POINT('Origin',(5.,3.5,0.));
#16303=CARTESIAN_POINT('Origin',(27.,-3.5,-1.3));
#16304=CARTESIAN_POINT('',(26.725,-3.5,-1.2));
#16305=CARTESIAN_POINT('Origin',(27.,-3.5,-1.2));
#16306=CARTESIAN_POINT('',(26.725,-3.5,0.));
#16307=CARTESIAN_POINT('',(26.725,-3.5,-1.3));
#16308=CARTESIAN_POINT('Origin',(27.,-3.5,0.));
#16309=CARTESIAN_POINT('Origin',(5.,-3.5,-1.3));
#16310=CARTESIAN_POINT('',(4.725,-3.5,-1.2));
#16311=CARTESIAN_POINT('Origin',(5.,-3.5,-1.2));
#16312=CARTESIAN_POINT('',(4.725,-3.5,0.));
#16313=CARTESIAN_POINT('',(4.725,-3.5,-1.3));
#16314=CARTESIAN_POINT('Origin',(5.,-3.5,0.));
#16315=CARTESIAN_POINT('Origin',(34.8,-1.,-1.1));
#16316=CARTESIAN_POINT('',(34.635,-1.,-1.1));
#16317=CARTESIAN_POINT('Origin',(34.8,-1.,-1.1));
#16318=CARTESIAN_POINT('',(34.635,-1.,0.));
#16319=CARTESIAN_POINT('',(34.635,-1.,-1.1));
#16320=CARTESIAN_POINT('Origin',(34.8,-1.,0.));
#16321=CARTESIAN_POINT('Origin',(34.8,-1.,-1.1));
#16322=CARTESIAN_POINT('Origin',(29.2,1.,-1.1));
#16323=CARTESIAN_POINT('',(29.035,1.,-1.1));
#16324=CARTESIAN_POINT('Origin',(29.2,1.,-1.1));
#16325=CARTESIAN_POINT('',(29.035,1.,0.));
#16326=CARTESIAN_POINT('',(29.035,1.,-1.1));
#16327=CARTESIAN_POINT('Origin',(29.2,1.,0.));
#16328=CARTESIAN_POINT('Origin',(29.2,1.,-1.1));
#16329=CARTESIAN_POINT('Origin',(29.2,-1.,-1.1));
#16330=CARTESIAN_POINT('',(29.035,-1.,-1.1));
#16331=CARTESIAN_POINT('Origin',(29.2,-1.,-1.1));
#16332=CARTESIAN_POINT('',(29.035,-1.,0.));
#16333=CARTESIAN_POINT('',(29.035,-1.,-1.1));
#16334=CARTESIAN_POINT('Origin',(29.2,-1.,0.));
#16335=CARTESIAN_POINT('Origin',(29.2,-1.,-1.1));
#16336=CARTESIAN_POINT('Origin',(34.8,1.,-1.1));
#16337=CARTESIAN_POINT('',(34.635,1.,-1.1));
#16338=CARTESIAN_POINT('Origin',(34.8,1.,-1.1));
#16339=CARTESIAN_POINT('',(34.635,1.,0.));
#16340=CARTESIAN_POINT('',(34.635,1.,-1.1));
#16341=CARTESIAN_POINT('Origin',(34.8,1.,0.));
#16342=CARTESIAN_POINT('Origin',(34.8,1.,-1.1));
#16343=CARTESIAN_POINT('Origin',(2.8,-1.,-1.1));
#16344=CARTESIAN_POINT('',(2.635,-1.,-1.1));
#16345=CARTESIAN_POINT('Origin',(2.8,-1.,-1.1));
#16346=CARTESIAN_POINT('',(2.635,-1.,0.));
#16347=CARTESIAN_POINT('',(2.635,-1.,-1.1));
#16348=CARTESIAN_POINT('Origin',(2.8,-1.,0.));
#16349=CARTESIAN_POINT('Origin',(2.8,-1.,-1.1));
#16350=CARTESIAN_POINT('Origin',(-2.8,1.,-1.1));
#16351=CARTESIAN_POINT('',(-2.965,1.,-1.1));
#16352=CARTESIAN_POINT('Origin',(-2.8,1.,-1.1));
#16353=CARTESIAN_POINT('',(-2.965,1.,0.));
#16354=CARTESIAN_POINT('',(-2.965,1.,-1.1));
#16355=CARTESIAN_POINT('Origin',(-2.8,1.,0.));
#16356=CARTESIAN_POINT('Origin',(-2.8,1.,-1.1));
#16357=CARTESIAN_POINT('Origin',(-2.8,-1.,-1.1));
#16358=CARTESIAN_POINT('',(-2.965,-1.,-1.1));
#16359=CARTESIAN_POINT('Origin',(-2.8,-1.,-1.1));
#16360=CARTESIAN_POINT('',(-2.965,-1.,0.));
#16361=CARTESIAN_POINT('',(-2.965,-1.,-1.1));
#16362=CARTESIAN_POINT('Origin',(-2.8,-1.,0.));
#16363=CARTESIAN_POINT('Origin',(-2.8,-1.,-1.1));
#16364=CARTESIAN_POINT('Origin',(2.8,1.,-1.1));
#16365=CARTESIAN_POINT('',(2.635,1.,-1.1));
#16366=CARTESIAN_POINT('Origin',(2.8,1.,-1.1));
#16367=CARTESIAN_POINT('',(2.635,1.,0.));
#16368=CARTESIAN_POINT('',(2.635,1.,-1.1));
#16369=CARTESIAN_POINT('Origin',(2.8,1.,0.));
#16370=CARTESIAN_POINT('Origin',(2.8,1.,-1.1));
#16371=CARTESIAN_POINT('Origin',(36.,4.5,-1.2));
#16372=CARTESIAN_POINT('',(36.,4.5,-1.2));
#16373=CARTESIAN_POINT('',(-4.,4.5,-1.2));
#16374=CARTESIAN_POINT('',(36.,4.5,-1.2));
#16375=CARTESIAN_POINT('',(-4.,4.5,0.));
#16376=CARTESIAN_POINT('',(-4.,4.5,-1.2));
#16377=CARTESIAN_POINT('',(36.,4.5,0.));
#16378=CARTESIAN_POINT('',(36.,4.5,0.));
#16379=CARTESIAN_POINT('',(36.,4.5,-1.2));
#16380=CARTESIAN_POINT('Origin',(36.,-6.5,-1.2));
#16381=CARTESIAN_POINT('',(36.,-6.5,-1.2));
#16382=CARTESIAN_POINT('',(36.,-6.5,-1.2));
#16383=CARTESIAN_POINT('',(36.,-6.5,0.));
#16384=CARTESIAN_POINT('',(36.,-6.5,0.));
#16385=CARTESIAN_POINT('',(36.,-6.5,-1.2));
#16386=CARTESIAN_POINT('Origin',(-4.,-6.5,-1.2));
#16387=CARTESIAN_POINT('',(-4.,-6.5,-1.2));
#16388=CARTESIAN_POINT('',(-4.,-6.5,-1.2));
#16389=CARTESIAN_POINT('',(-4.,-6.5,0.));
#16390=CARTESIAN_POINT('',(-4.,-6.5,0.));
#16391=CARTESIAN_POINT('',(-4.,-6.5,-1.2));
#16392=CARTESIAN_POINT('Origin',(-4.,4.5,-1.2));
#16393=CARTESIAN_POINT('',(-4.,4.5,-1.2));
#16394=CARTESIAN_POINT('',(-4.,4.5,0.));
#16395=CARTESIAN_POINT('Origin',(16.,-1.,0.));
#16396=CARTESIAN_POINT('Origin',(16.,-1.,-1.2));
#16397=CARTESIAN_POINT('',(0.,0.,0.));
#16398=CARTESIAN_POINT('Origin',(-4.1,2.49,-2.5));
#16399=CARTESIAN_POINT('',(-4.,2.49,-2.4));
#16400=CARTESIAN_POINT('',(-3.,2.49,-2.4));
#16401=CARTESIAN_POINT('',(-3.8,2.49,-2.4));
#16402=CARTESIAN_POINT('',(-4.,2.49,-1.2));
#16403=CARTESIAN_POINT('',(-4.,2.49,-2.45));
#16404=CARTESIAN_POINT('',(-3.,2.49,-1.2));
#16405=CARTESIAN_POINT('',(-3.8,2.49,-1.2));
#16406=CARTESIAN_POINT('',(-3.,2.49,-2.45));
#16407=CARTESIAN_POINT('Origin',(-3.5,-1.,-1.2));
#16408=CARTESIAN_POINT('',(-4.,-2.49,-1.2));
#16409=CARTESIAN_POINT('',(-4.,4.5,-1.2));
#16410=CARTESIAN_POINT('',(-3.,-2.49,-1.2));
#16411=CARTESIAN_POINT('',(16.3,-2.49,-1.2));
#16412=CARTESIAN_POINT('',(-3.,-6.5,-1.2));
#16413=CARTESIAN_POINT('Origin',(-4.,4.5,-2.4));
#16414=CARTESIAN_POINT('',(-4.,-2.49,-2.4));
#16415=CARTESIAN_POINT('',(-4.,4.5,-2.4));
#16416=CARTESIAN_POINT('',(-4.,-2.49,-2.45));
#16417=CARTESIAN_POINT('Origin',(36.1,-2.49,-2.5));
#16418=CARTESIAN_POINT('',(-3.,-2.49,-2.4));
#16419=CARTESIAN_POINT('',(16.3,-2.49,-2.4));
#16420=CARTESIAN_POINT('',(-3.,-2.49,-2.45));
#16421=CARTESIAN_POINT('Origin',(-3.5,-1.,-2.4));
#16422=CARTESIAN_POINT('',(-3.,-6.5,-2.4));
#16423=CARTESIAN_POINT('Origin',(-3.,-6.5,-2.4));
#16424=CARTESIAN_POINT('Origin',(-4.,-6.5,-2.4));
#16425=CARTESIAN_POINT('',(-4.,-6.5,-2.4));
#16426=CARTESIAN_POINT('',(-3.,-6.5,-2.4));
#16427=CARTESIAN_POINT('',(-4.,-6.5,-2.4));
#16428=CARTESIAN_POINT('',(-3.,-6.5,-1.2));
#16429=CARTESIAN_POINT('',(-3.,-6.5,-2.4));
#16430=CARTESIAN_POINT('',(-4.,-6.5,-1.2));
#16431=CARTESIAN_POINT('',(-4.,-6.5,-1.2));
#16432=CARTESIAN_POINT('',(-4.,-6.5,-2.4));
#16433=CARTESIAN_POINT('Origin',(-4.,4.5,-2.4));
#16434=CARTESIAN_POINT('',(-4.,-4.51,-1.2));
#16435=CARTESIAN_POINT('',(-4.,-4.51,-2.4));
#16436=CARTESIAN_POINT('',(-4.,-4.51,-2.45));
#16437=CARTESIAN_POINT('',(-4.,4.5,-2.4));
#16438=CARTESIAN_POINT('',(-4.,4.5,-1.2));
#16439=CARTESIAN_POINT('Origin',(-3.5,-1.,-1.2));
#16440=CARTESIAN_POINT('',(-3.,-4.51,-1.2));
#16441=CARTESIAN_POINT('',(-3.8,-4.51,-1.2));
#16442=CARTESIAN_POINT('',(-3.,-6.5,-1.2));
#16443=CARTESIAN_POINT('Origin',(-3.,-6.5,-2.4));
#16444=CARTESIAN_POINT('',(-3.,-4.51,-2.4));
#16445=CARTESIAN_POINT('',(-3.,-4.51,-2.45));
#16446=CARTESIAN_POINT('',(-3.,-6.5,-2.4));
#16447=CARTESIAN_POINT('Origin',(-3.5,-1.,-2.4));
#16448=CARTESIAN_POINT('',(-3.8,-4.51,-2.4));
#16449=CARTESIAN_POINT('Origin',(-4.1,-4.51,-2.5));
#16450=CARTESIAN_POINT('',(0.,0.,0.));
#16451=CARTESIAN_POINT('Origin',(-4.1,2.49,-2.5));
#16452=CARTESIAN_POINT('',(35.,2.49,-2.4));
#16453=CARTESIAN_POINT('',(36.,2.49,-2.4));
#16454=CARTESIAN_POINT('',(15.7,2.49,-2.4));
#16455=CARTESIAN_POINT('',(35.,2.49,-1.2));
#16456=CARTESIAN_POINT('',(35.,2.49,-2.45));
#16457=CARTESIAN_POINT('',(36.,2.49,-1.2));
#16458=CARTESIAN_POINT('',(15.7,2.49,-1.2));
#16459=CARTESIAN_POINT('',(36.,2.49,-2.45));
#16460=CARTESIAN_POINT('Origin',(35.5,-1.,-1.2));
#16461=CARTESIAN_POINT('',(35.,-2.49,-1.2));
#16462=CARTESIAN_POINT('',(35.,4.5,-1.2));
#16463=CARTESIAN_POINT('',(36.,-2.49,-1.2));
#16464=CARTESIAN_POINT('',(35.8,-2.49,-1.2));
#16465=CARTESIAN_POINT('',(36.,-6.5,-1.2));
#16466=CARTESIAN_POINT('Origin',(35.,4.5,-2.4));
#16467=CARTESIAN_POINT('',(35.,-2.49,-2.4));
#16468=CARTESIAN_POINT('',(35.,4.5,-2.4));
#16469=CARTESIAN_POINT('',(35.,-2.49,-2.45));
#16470=CARTESIAN_POINT('Origin',(36.1,-2.49,-2.5));
#16471=CARTESIAN_POINT('',(36.,-2.49,-2.4));
#16472=CARTESIAN_POINT('',(35.8,-2.49,-2.4));
#16473=CARTESIAN_POINT('',(36.,-2.49,-2.45));
#16474=CARTESIAN_POINT('Origin',(35.5,-1.,-2.4));
#16475=CARTESIAN_POINT('',(36.,-6.5,-2.4));
#16476=CARTESIAN_POINT('Origin',(36.,-6.5,-2.4));
#16477=CARTESIAN_POINT('Origin',(35.,-6.5,-2.4));
#16478=CARTESIAN_POINT('',(35.,-6.5,-2.4));
#16479=CARTESIAN_POINT('',(36.,-6.5,-2.4));
#16480=CARTESIAN_POINT('',(35.,-6.5,-2.4));
#16481=CARTESIAN_POINT('',(36.,-6.5,-1.2));
#16482=CARTESIAN_POINT('',(36.,-6.5,-2.4));
#16483=CARTESIAN_POINT('',(35.,-6.5,-1.2));
#16484=CARTESIAN_POINT('',(35.,-6.5,-1.2));
#16485=CARTESIAN_POINT('',(35.,-6.5,-2.4));
#16486=CARTESIAN_POINT('Origin',(35.,4.5,-2.4));
#16487=CARTESIAN_POINT('',(35.,-4.51,-1.2));
#16488=CARTESIAN_POINT('',(35.,-4.51,-2.4));
#16489=CARTESIAN_POINT('',(35.,-4.51,-2.45));
#16490=CARTESIAN_POINT('',(35.,4.5,-2.4));
#16491=CARTESIAN_POINT('',(35.,4.5,-1.2));
#16492=CARTESIAN_POINT('Origin',(35.5,-1.,-1.2));
#16493=CARTESIAN_POINT('',(36.,-4.51,-1.2));
#16494=CARTESIAN_POINT('',(15.7,-4.51,-1.2));
#16495=CARTESIAN_POINT('',(36.,-6.5,-1.2));
#16496=CARTESIAN_POINT('Origin',(36.,-6.5,-2.4));
#16497=CARTESIAN_POINT('',(36.,-4.51,-2.4));
#16498=CARTESIAN_POINT('',(36.,-4.51,-2.45));
#16499=CARTESIAN_POINT('',(36.,-6.5,-2.4));
#16500=CARTESIAN_POINT('Origin',(35.5,-1.,-2.4));
#16501=CARTESIAN_POINT('',(15.7,-4.51,-2.4));
#16502=CARTESIAN_POINT('Origin',(-4.1,-4.51,-2.5));
#16503=CARTESIAN_POINT('',(0.,0.,0.));
#16504=CARTESIAN_POINT('Origin',(-1.34350288425444,-1.9,5.65649711574556));
#16505=CARTESIAN_POINT('',(-1.50850288425444,-1.8,5.65649711574556));
#16506=CARTESIAN_POINT('Origin',(-1.34350288425444,-1.8,5.65649711574556));
#16507=CARTESIAN_POINT('',(-1.50850288425444,1.8,5.65649711574556));
#16508=CARTESIAN_POINT('',(-1.50850288425444,-1.9,5.65649711574556));
#16509=CARTESIAN_POINT('Origin',(-1.34350288425444,1.8,5.65649711574556));
#16510=CARTESIAN_POINT('Origin',(-1.34350288425444,-1.9,8.34350288425444));
#16511=CARTESIAN_POINT('',(-1.50850288425444,-1.8,8.34350288425444));
#16512=CARTESIAN_POINT('Origin',(-1.34350288425444,-1.8,8.34350288425444));
#16513=CARTESIAN_POINT('',(-1.50850288425444,1.8,8.34350288425444));
#16514=CARTESIAN_POINT('',(-1.50850288425444,-1.9,8.34350288425444));
#16515=CARTESIAN_POINT('Origin',(-1.34350288425444,1.8,8.34350288425444));
#16516=CARTESIAN_POINT('Origin',(1.34350288425444,-1.9,8.34350288425444));
#16517=CARTESIAN_POINT('',(1.17850288425444,-1.8,8.34350288425444));
#16518=CARTESIAN_POINT('Origin',(1.34350288425444,-1.8,8.34350288425444));
#16519=CARTESIAN_POINT('',(1.17850288425444,1.8,8.34350288425444));
#16520=CARTESIAN_POINT('',(1.17850288425444,-1.9,8.34350288425444));
#16521=CARTESIAN_POINT('Origin',(1.34350288425444,1.8,8.34350288425444));
#16522=CARTESIAN_POINT('Origin',(1.34350288425444,-1.9,5.65649711574556));
#16523=CARTESIAN_POINT('',(1.17850288425444,-1.8,5.65649711574556));
#16524=CARTESIAN_POINT('Origin',(1.34350288425444,-1.8,5.65649711574556));
#16525=CARTESIAN_POINT('',(1.17850288425444,1.8,5.65649711574556));
#16526=CARTESIAN_POINT('',(1.17850288425444,-1.9,5.65649711574556));
#16527=CARTESIAN_POINT('Origin',(1.34350288425444,1.8,5.65649711574556));
#16528=CARTESIAN_POINT('Origin',(0.,-1.9,7.));
#16529=CARTESIAN_POINT('',(-1.5,-1.8,7.));
#16530=CARTESIAN_POINT('Origin',(0.,-1.8,7.));
#16531=CARTESIAN_POINT('',(-1.5,1.8,7.));
#16532=CARTESIAN_POINT('',(-1.5,-1.9,7.));
#16533=CARTESIAN_POINT('Origin',(0.,1.8,7.));
#16534=CARTESIAN_POINT('Origin',(2.8,-1.,-0.1));
#16535=CARTESIAN_POINT('',(2.575,-1.,0.));
#16536=CARTESIAN_POINT('Origin',(2.8,-1.,0.));
#16537=CARTESIAN_POINT('',(2.575,-1.,0.8));
#16538=CARTESIAN_POINT('',(2.575,-1.,-0.1));
#16539=CARTESIAN_POINT('Origin',(2.8,-1.,0.8));
#16540=CARTESIAN_POINT('Origin',(-2.8,1.,-0.1));
#16541=CARTESIAN_POINT('',(-3.025,1.,0.));
#16542=CARTESIAN_POINT('Origin',(-2.8,1.,0.));
#16543=CARTESIAN_POINT('',(-3.025,1.,0.8));
#16544=CARTESIAN_POINT('',(-3.025,1.,-0.1));
#16545=CARTESIAN_POINT('Origin',(-2.8,1.,0.8));
#16546=CARTESIAN_POINT('Origin',(-2.8,-1.,-0.1));
#16547=CARTESIAN_POINT('',(-3.025,-1.,0.));
#16548=CARTESIAN_POINT('Origin',(-2.8,-1.,0.));
#16549=CARTESIAN_POINT('',(-3.025,-1.,0.8));
#16550=CARTESIAN_POINT('',(-3.025,-1.,-0.1));
#16551=CARTESIAN_POINT('Origin',(-2.8,-1.,0.8));
#16552=CARTESIAN_POINT('Origin',(2.8,1.,-0.1));
#16553=CARTESIAN_POINT('',(2.575,1.,0.));
#16554=CARTESIAN_POINT('Origin',(2.8,1.,0.));
#16555=CARTESIAN_POINT('',(2.575,1.,0.8));
#16556=CARTESIAN_POINT('',(2.575,1.,-0.1));
#16557=CARTESIAN_POINT('Origin',(2.8,1.,0.8));
#16558=CARTESIAN_POINT('Origin',(-3.4,-1.8,0.8));
#16559=CARTESIAN_POINT('',(2.2,-1.8,0.8));
#16560=CARTESIAN_POINT('',(2.2,1.8,0.8));
#16561=CARTESIAN_POINT('',(2.2,-1.8,0.8));
#16562=CARTESIAN_POINT('',(3.4,-1.8,0.8));
#16563=CARTESIAN_POINT('',(3.4,-1.8,0.8));
#16564=CARTESIAN_POINT('',(3.4,1.8,0.8));
#16565=CARTESIAN_POINT('',(3.4,-1.8,0.8));
#16566=CARTESIAN_POINT('',(3.4,1.8,0.8));
#16567=CARTESIAN_POINT('Origin',(-3.4,-1.8,0.8));
#16568=CARTESIAN_POINT('',(-2.2,1.8,0.8));
#16569=CARTESIAN_POINT('',(-2.2,-1.8,0.8));
#16570=CARTESIAN_POINT('',(-2.2,0.,0.8));
#16571=CARTESIAN_POINT('',(-3.4,1.8,0.8));
#16572=CARTESIAN_POINT('',(3.4,1.8,0.8));
#16573=CARTESIAN_POINT('',(-3.4,-1.8,0.8));
#16574=CARTESIAN_POINT('',(-3.4,-1.8,0.8));
#16575=CARTESIAN_POINT('',(3.4,-1.8,0.8));
#16576=CARTESIAN_POINT('Origin',(-3.4,-1.8,0.));
#16577=CARTESIAN_POINT('',(-3.4,-1.8,0.));
#16578=CARTESIAN_POINT('',(-3.4,-1.8,0.8));
#16579=CARTESIAN_POINT('',(-3.4,1.8,0.));
#16580=CARTESIAN_POINT('',(-3.4,1.8,0.8));
#16581=CARTESIAN_POINT('',(-3.4,-1.8,0.));
#16582=CARTESIAN_POINT('Origin',(3.4,-1.8,0.8));
#16583=CARTESIAN_POINT('',(3.4,-1.8,0.));
#16584=CARTESIAN_POINT('',(3.4,-1.8,0.));
#16585=CARTESIAN_POINT('',(3.4,1.8,0.));
#16586=CARTESIAN_POINT('',(3.4,-1.8,0.));
#16587=CARTESIAN_POINT('',(3.4,1.8,0.));
#16588=CARTESIAN_POINT('Origin',(-2.2,-1.8,0.));
#16589=CARTESIAN_POINT('',(2.2,-1.8,9.2));
#16590=CARTESIAN_POINT('',(2.2,-1.8,0.));
#16591=CARTESIAN_POINT('',(-2.2,-1.8,9.2));
#16592=CARTESIAN_POINT('',(-2.2,-1.8,9.2));
#16593=CARTESIAN_POINT('',(-2.2,-1.8,0.));
#16594=CARTESIAN_POINT('',(-3.4,-1.8,0.));
#16595=CARTESIAN_POINT('Origin',(2.2,-1.8,0.));
#16596=CARTESIAN_POINT('',(2.2,1.8,9.2));
#16597=CARTESIAN_POINT('',(2.2,1.8,0.));
#16598=CARTESIAN_POINT('',(2.2,-1.8,9.2));
#16599=CARTESIAN_POINT('Origin',(2.2,1.8,0.));
#16600=CARTESIAN_POINT('',(-2.2,1.8,9.2));
#16601=CARTESIAN_POINT('',(-2.2,1.8,0.));
#16602=CARTESIAN_POINT('',(2.2,1.8,9.2));
#16603=CARTESIAN_POINT('',(-3.4,1.8,0.));
#16604=CARTESIAN_POINT('Origin',(-2.2,1.8,0.));
#16605=CARTESIAN_POINT('',(-2.2,1.8,9.2));
#16606=CARTESIAN_POINT('Origin',(0.,0.,9.2));
#16607=CARTESIAN_POINT('Origin',(0.,0.,0.));
#16608=CARTESIAN_POINT('',(0.,0.,0.));
#16609=CARTESIAN_POINT('Origin',(0.,-0.45,7.));
#16610=CARTESIAN_POINT('',(-1.1,0.45,7.));
#16611=CARTESIAN_POINT('Origin',(0.,0.45,7.));
#16612=CARTESIAN_POINT('',(-1.1,-0.45,7.));
#16613=CARTESIAN_POINT('',(-1.1,-0.45,7.));
#16614=CARTESIAN_POINT('Origin',(0.,-0.45,7.));
#16615=CARTESIAN_POINT('Origin',(0.,-0.45,7.));
#16616=CARTESIAN_POINT('',(-1.49,0.45,7.));
#16617=CARTESIAN_POINT('Origin',(0.,0.45,7.));
#16618=CARTESIAN_POINT('',(-1.49,-0.45,7.));
#16619=CARTESIAN_POINT('',(-1.49,-0.45,7.));
#16620=CARTESIAN_POINT('Origin',(0.,-0.45,7.));
#16621=CARTESIAN_POINT('Origin',(0.,0.45,7.));
#16622=CARTESIAN_POINT('Origin',(0.,-0.45,7.));
#16623=CARTESIAN_POINT('',(0.,0.,0.));
#16624=CARTESIAN_POINT('Origin',(-1.34350288425444,-2.2,5.65649711574556));
#16625=CARTESIAN_POINT('',(-1.40634555589641,-2.1,5.4404512904656));
#16626=CARTESIAN_POINT('',(-1.40634555589641,-1.8,5.4404512904656));
#16627=CARTESIAN_POINT('',(-1.40634555589641,-2.2,5.4404512904656));
#16628=CARTESIAN_POINT('',(-1.5595487095344,-2.1,5.59365444410359));
#16629=CARTESIAN_POINT('Origin',(-1.34350288425444,-2.1,5.65649711574556));
#16630=CARTESIAN_POINT('',(-1.5595487095344,-1.8,5.59365444410359));
#16631=CARTESIAN_POINT('',(-1.5595487095344,-2.2,5.59365444410359));
#16632=CARTESIAN_POINT('Origin',(-1.34350288425444,-1.8,5.65649711574556));
#16633=CARTESIAN_POINT('Origin',(-1.34350288425444,-2.2,8.34350288425444));
#16634=CARTESIAN_POINT('',(-1.5595487095344,-2.1,8.40634555589641));
#16635=CARTESIAN_POINT('',(-1.5595487095344,-1.8,8.40634555589641));
#16636=CARTESIAN_POINT('',(-1.5595487095344,-2.2,8.40634555589641));
#16637=CARTESIAN_POINT('',(-1.40634555589641,-2.1,8.5595487095344));
#16638=CARTESIAN_POINT('Origin',(-1.34350288425444,-2.1,8.34350288425444));
#16639=CARTESIAN_POINT('',(-1.40634555589641,-1.8,8.5595487095344));
#16640=CARTESIAN_POINT('',(-1.40634555589641,-2.2,8.5595487095344));
#16641=CARTESIAN_POINT('Origin',(-1.34350288425444,-1.8,8.34350288425444));
#16642=CARTESIAN_POINT('Origin',(1.34350288425444,-2.2,8.34350288425444));
#16643=CARTESIAN_POINT('',(1.40634555589641,-2.1,8.5595487095344));
#16644=CARTESIAN_POINT('',(1.40634555589641,-1.8,8.5595487095344));
#16645=CARTESIAN_POINT('',(1.40634555589641,-2.2,8.5595487095344));
#16646=CARTESIAN_POINT('',(1.5595487095344,-2.1,8.40634555589641));
#16647=CARTESIAN_POINT('Origin',(1.34350288425444,-2.1,8.34350288425444));
#16648=CARTESIAN_POINT('',(1.5595487095344,-1.8,8.40634555589641));
#16649=CARTESIAN_POINT('',(1.5595487095344,-2.2,8.40634555589641));
#16650=CARTESIAN_POINT('Origin',(1.34350288425444,-1.8,8.34350288425444));
#16651=CARTESIAN_POINT('Origin',(1.34350288425444,-2.2,5.65649711574556));
#16652=CARTESIAN_POINT('',(1.5595487095344,-2.1,5.59365444410359));
#16653=CARTESIAN_POINT('',(1.5595487095344,-1.8,5.59365444410359));
#16654=CARTESIAN_POINT('',(1.5595487095344,-2.2,5.59365444410359));
#16655=CARTESIAN_POINT('',(1.40634555589641,-2.1,5.4404512904656));
#16656=CARTESIAN_POINT('Origin',(1.34350288425444,-2.1,5.65649711574556));
#16657=CARTESIAN_POINT('',(1.40634555589641,-1.8,5.4404512904656));
#16658=CARTESIAN_POINT('',(1.40634555589641,-2.2,5.4404512904656));
#16659=CARTESIAN_POINT('Origin',(1.34350288425444,-1.8,5.65649711574556));
#16660=CARTESIAN_POINT('Origin',(0.,-2.1,7.));
#16661=CARTESIAN_POINT('Origin',(0.,-2.1,7.));
#16662=CARTESIAN_POINT('Origin',(0.,-2.1,7.));
#16663=CARTESIAN_POINT('Origin',(0.,-2.1,7.));
#16664=CARTESIAN_POINT('Origin',(0.,-2.1,7.));
#16665=CARTESIAN_POINT('',(-1.1,-2.1,7.));
#16666=CARTESIAN_POINT('Origin',(0.,-2.1,7.));
#16667=CARTESIAN_POINT('Origin',(0.,-2.1,7.));
#16668=CARTESIAN_POINT('Origin',(0.,-1.8,7.));
#16669=CARTESIAN_POINT('Origin',(0.,-2.1,7.));
#16670=CARTESIAN_POINT('Origin',(0.,-1.8,7.));
#16671=CARTESIAN_POINT('Origin',(0.,-2.1,7.));
#16672=CARTESIAN_POINT('Origin',(0.,-1.8,7.));
#16673=CARTESIAN_POINT('Origin',(0.,-2.1,7.));
#16674=CARTESIAN_POINT('Origin',(0.,-1.8,7.));
#16675=CARTESIAN_POINT('Origin',(0.,-1.8,7.));
#16676=CARTESIAN_POINT('',(-1.49,-1.35,7.));
#16677=CARTESIAN_POINT('Origin',(0.,-1.35,7.));
#16678=CARTESIAN_POINT('',(-1.49,-1.8,7.));
#16679=CARTESIAN_POINT('',(-1.49,-1.8,7.));
#16680=CARTESIAN_POINT('Origin',(0.,-1.8,7.));
#16681=CARTESIAN_POINT('Origin',(0.,-1.35,7.));
#16682=CARTESIAN_POINT('',(-1.1,-1.35,7.));
#16683=CARTESIAN_POINT('Origin',(0.,-1.35,7.));
#16684=CARTESIAN_POINT('Origin',(0.,-2.1,7.));
#16685=CARTESIAN_POINT('',(-1.1,-2.1,7.));
#16686=CARTESIAN_POINT('Origin',(0.,-1.8,7.));
#16687=CARTESIAN_POINT('',(0.,0.,0.));
#16688=CARTESIAN_POINT('Origin',(-1.34350288425444,1.7,5.65649711574556));
#16689=CARTESIAN_POINT('',(-1.40634555589641,1.8,5.4404512904656));
#16690=CARTESIAN_POINT('',(-1.40634555589641,2.1,5.4404512904656));
#16691=CARTESIAN_POINT('',(-1.40634555589641,1.7,5.4404512904656));
#16692=CARTESIAN_POINT('',(-1.5595487095344,1.8,5.59365444410359));
#16693=CARTESIAN_POINT('Origin',(-1.34350288425444,1.8,5.65649711574556));
#16694=CARTESIAN_POINT('',(-1.5595487095344,2.1,5.59365444410359));
#16695=CARTESIAN_POINT('',(-1.5595487095344,1.7,5.59365444410359));
#16696=CARTESIAN_POINT('Origin',(-1.34350288425444,2.1,5.65649711574556));
#16697=CARTESIAN_POINT('Origin',(-1.34350288425444,1.7,8.34350288425444));
#16698=CARTESIAN_POINT('',(-1.5595487095344,1.8,8.40634555589641));
#16699=CARTESIAN_POINT('',(-1.5595487095344,2.1,8.40634555589641));
#16700=CARTESIAN_POINT('',(-1.5595487095344,1.7,8.40634555589641));
#16701=CARTESIAN_POINT('',(-1.40634555589641,1.8,8.5595487095344));
#16702=CARTESIAN_POINT('Origin',(-1.34350288425444,1.8,8.34350288425444));
#16703=CARTESIAN_POINT('',(-1.40634555589641,2.1,8.5595487095344));
#16704=CARTESIAN_POINT('',(-1.40634555589641,1.7,8.5595487095344));
#16705=CARTESIAN_POINT('Origin',(-1.34350288425444,2.1,8.34350288425444));
#16706=CARTESIAN_POINT('Origin',(1.34350288425444,1.7,8.34350288425444));
#16707=CARTESIAN_POINT('',(1.40634555589641,1.8,8.5595487095344));
#16708=CARTESIAN_POINT('',(1.40634555589641,2.1,8.5595487095344));
#16709=CARTESIAN_POINT('',(1.40634555589641,1.7,8.5595487095344));
#16710=CARTESIAN_POINT('',(1.5595487095344,1.8,8.40634555589641));
#16711=CARTESIAN_POINT('Origin',(1.34350288425444,1.8,8.34350288425444));
#16712=CARTESIAN_POINT('',(1.5595487095344,2.1,8.40634555589641));
#16713=CARTESIAN_POINT('',(1.5595487095344,1.7,8.40634555589641));
#16714=CARTESIAN_POINT('Origin',(1.34350288425444,2.1,8.34350288425444));
#16715=CARTESIAN_POINT('Origin',(1.34350288425444,1.7,5.65649711574556));
#16716=CARTESIAN_POINT('',(1.5595487095344,1.8,5.59365444410359));
#16717=CARTESIAN_POINT('',(1.5595487095344,2.1,5.59365444410359));
#16718=CARTESIAN_POINT('',(1.5595487095344,1.7,5.59365444410359));
#16719=CARTESIAN_POINT('',(1.40634555589641,1.8,5.4404512904656));
#16720=CARTESIAN_POINT('Origin',(1.34350288425444,1.8,5.65649711574556));
#16721=CARTESIAN_POINT('',(1.40634555589641,2.1,5.4404512904656));
#16722=CARTESIAN_POINT('',(1.40634555589641,1.7,5.4404512904656));
#16723=CARTESIAN_POINT('Origin',(1.34350288425444,2.1,5.65649711574556));
#16724=CARTESIAN_POINT('Origin',(0.,1.8,7.));
#16725=CARTESIAN_POINT('Origin',(0.,1.8,7.));
#16726=CARTESIAN_POINT('Origin',(0.,1.8,7.));
#16727=CARTESIAN_POINT('Origin',(0.,1.8,7.));
#16728=CARTESIAN_POINT('Origin',(0.,1.8,7.));
#16729=CARTESIAN_POINT('',(-1.49,1.8,7.));
#16730=CARTESIAN_POINT('Origin',(0.,1.8,7.));
#16731=CARTESIAN_POINT('Origin',(0.,1.8,7.));
#16732=CARTESIAN_POINT('Origin',(0.,2.1,7.));
#16733=CARTESIAN_POINT('Origin',(0.,1.8,7.));
#16734=CARTESIAN_POINT('Origin',(0.,2.1,7.));
#16735=CARTESIAN_POINT('Origin',(0.,1.8,7.));
#16736=CARTESIAN_POINT('Origin',(0.,2.1,7.));
#16737=CARTESIAN_POINT('Origin',(0.,1.8,7.));
#16738=CARTESIAN_POINT('Origin',(0.,2.1,7.));
#16739=CARTESIAN_POINT('Origin',(0.,1.35,7.));
#16740=CARTESIAN_POINT('',(-1.49,1.35,7.));
#16741=CARTESIAN_POINT('',(-1.49,1.35,7.));
#16742=CARTESIAN_POINT('Origin',(0.,1.35,7.));
#16743=CARTESIAN_POINT('Origin',(0.,1.35,7.));
#16744=CARTESIAN_POINT('',(-1.1,1.35,7.));
#16745=CARTESIAN_POINT('Origin',(0.,1.35,7.));
#16746=CARTESIAN_POINT('Origin',(0.,1.8,7.));
#16747=CARTESIAN_POINT('',(-1.1,2.1,7.));
#16748=CARTESIAN_POINT('Origin',(0.,2.1,7.));
#16749=CARTESIAN_POINT('',(-1.1,1.8,7.));
#16750=CARTESIAN_POINT('Origin',(0.,2.1,7.));
#16751=CARTESIAN_POINT('',(0.,0.,0.));
#16752=CARTESIAN_POINT('Origin',(30.6564971157456,-1.9,5.65649711574556));
#16753=CARTESIAN_POINT('',(30.4914971157456,-1.8,5.65649711574556));
#16754=CARTESIAN_POINT('Origin',(30.6564971157456,-1.8,5.65649711574556));
#16755=CARTESIAN_POINT('',(30.4914971157456,1.8,5.65649711574556));
#16756=CARTESIAN_POINT('',(30.4914971157456,-1.9,5.65649711574556));
#16757=CARTESIAN_POINT('Origin',(30.6564971157456,1.8,5.65649711574556));
#16758=CARTESIAN_POINT('Origin',(30.6564971157456,-1.9,8.34350288425444));
#16759=CARTESIAN_POINT('',(30.4914971157456,-1.8,8.34350288425444));
#16760=CARTESIAN_POINT('Origin',(30.6564971157456,-1.8,8.34350288425444));
#16761=CARTESIAN_POINT('',(30.4914971157456,1.8,8.34350288425444));
#16762=CARTESIAN_POINT('',(30.4914971157456,-1.9,8.34350288425444));
#16763=CARTESIAN_POINT('Origin',(30.6564971157456,1.8,8.34350288425444));
#16764=CARTESIAN_POINT('Origin',(33.3435028842544,-1.9,8.34350288425444));
#16765=CARTESIAN_POINT('',(33.1785028842544,-1.8,8.34350288425444));
#16766=CARTESIAN_POINT('Origin',(33.3435028842544,-1.8,8.34350288425444));
#16767=CARTESIAN_POINT('',(33.1785028842544,1.8,8.34350288425444));
#16768=CARTESIAN_POINT('',(33.1785028842544,-1.9,8.34350288425444));
#16769=CARTESIAN_POINT('Origin',(33.3435028842544,1.8,8.34350288425444));
#16770=CARTESIAN_POINT('Origin',(33.3435028842544,-1.9,5.65649711574556));
#16771=CARTESIAN_POINT('',(33.1785028842544,-1.8,5.65649711574556));
#16772=CARTESIAN_POINT('Origin',(33.3435028842544,-1.8,5.65649711574556));
#16773=CARTESIAN_POINT('',(33.1785028842544,1.8,5.65649711574556));
#16774=CARTESIAN_POINT('',(33.1785028842544,-1.9,5.65649711574556));
#16775=CARTESIAN_POINT('Origin',(33.3435028842544,1.8,5.65649711574556));
#16776=CARTESIAN_POINT('Origin',(32.,-1.9,7.));
#16777=CARTESIAN_POINT('',(30.5,-1.8,7.));
#16778=CARTESIAN_POINT('Origin',(32.,-1.8,7.));
#16779=CARTESIAN_POINT('',(30.5,1.8,7.));
#16780=CARTESIAN_POINT('',(30.5,-1.9,7.));
#16781=CARTESIAN_POINT('Origin',(32.,1.8,7.));
#16782=CARTESIAN_POINT('Origin',(34.8,-1.,-0.1));
#16783=CARTESIAN_POINT('',(34.575,-1.,0.));
#16784=CARTESIAN_POINT('Origin',(34.8,-1.,0.));
#16785=CARTESIAN_POINT('',(34.575,-1.,0.8));
#16786=CARTESIAN_POINT('',(34.575,-1.,-0.1));
#16787=CARTESIAN_POINT('Origin',(34.8,-1.,0.8));
#16788=CARTESIAN_POINT('Origin',(29.2,1.,-0.1));
#16789=CARTESIAN_POINT('',(28.975,1.,0.));
#16790=CARTESIAN_POINT('Origin',(29.2,1.,0.));
#16791=CARTESIAN_POINT('',(28.975,1.,0.8));
#16792=CARTESIAN_POINT('',(28.975,1.,-0.1));
#16793=CARTESIAN_POINT('Origin',(29.2,1.,0.8));
#16794=CARTESIAN_POINT('Origin',(29.2,-1.,-0.1));
#16795=CARTESIAN_POINT('',(28.975,-1.,0.));
#16796=CARTESIAN_POINT('Origin',(29.2,-1.,0.));
#16797=CARTESIAN_POINT('',(28.975,-1.,0.8));
#16798=CARTESIAN_POINT('',(28.975,-1.,-0.1));
#16799=CARTESIAN_POINT('Origin',(29.2,-1.,0.8));
#16800=CARTESIAN_POINT('Origin',(34.8,1.,-0.1));
#16801=CARTESIAN_POINT('',(34.575,1.,0.));
#16802=CARTESIAN_POINT('Origin',(34.8,1.,0.));
#16803=CARTESIAN_POINT('',(34.575,1.,0.8));
#16804=CARTESIAN_POINT('',(34.575,1.,-0.1));
#16805=CARTESIAN_POINT('Origin',(34.8,1.,0.8));
#16806=CARTESIAN_POINT('Origin',(28.6,-1.8,0.8));
#16807=CARTESIAN_POINT('',(34.2,-1.8,0.8));
#16808=CARTESIAN_POINT('',(34.2,1.8,0.8));
#16809=CARTESIAN_POINT('',(34.2,-1.8,0.8));
#16810=CARTESIAN_POINT('',(35.4,-1.8,0.8));
#16811=CARTESIAN_POINT('',(35.4,-1.8,0.8));
#16812=CARTESIAN_POINT('',(35.4,1.8,0.8));
#16813=CARTESIAN_POINT('',(35.4,-1.8,0.8));
#16814=CARTESIAN_POINT('',(35.4,1.8,0.8));
#16815=CARTESIAN_POINT('Origin',(28.6,-1.8,0.8));
#16816=CARTESIAN_POINT('',(29.8,1.8,0.8));
#16817=CARTESIAN_POINT('',(29.8,-1.8,0.8));
#16818=CARTESIAN_POINT('',(29.8,0.,0.8));
#16819=CARTESIAN_POINT('',(28.6,1.8,0.8));
#16820=CARTESIAN_POINT('',(35.4,1.8,0.8));
#16821=CARTESIAN_POINT('',(28.6,-1.8,0.8));
#16822=CARTESIAN_POINT('',(28.6,-1.8,0.8));
#16823=CARTESIAN_POINT('',(35.4,-1.8,0.8));
#16824=CARTESIAN_POINT('Origin',(28.6,-1.8,0.));
#16825=CARTESIAN_POINT('',(28.6,-1.8,0.));
#16826=CARTESIAN_POINT('',(28.6,-1.8,0.8));
#16827=CARTESIAN_POINT('',(28.6,1.8,0.));
#16828=CARTESIAN_POINT('',(28.6,1.8,0.8));
#16829=CARTESIAN_POINT('',(28.6,-1.8,0.));
#16830=CARTESIAN_POINT('Origin',(35.4,-1.8,0.8));
#16831=CARTESIAN_POINT('',(35.4,-1.8,0.));
#16832=CARTESIAN_POINT('',(35.4,-1.8,0.));
#16833=CARTESIAN_POINT('',(35.4,1.8,0.));
#16834=CARTESIAN_POINT('',(35.4,-1.8,0.));
#16835=CARTESIAN_POINT('',(35.4,1.8,0.));
#16836=CARTESIAN_POINT('Origin',(29.8,-1.8,0.));
#16837=CARTESIAN_POINT('',(34.2,-1.8,9.2));
#16838=CARTESIAN_POINT('',(34.2,-1.8,0.));
#16839=CARTESIAN_POINT('',(29.8,-1.8,9.2));
#16840=CARTESIAN_POINT('',(29.8,-1.8,9.2));
#16841=CARTESIAN_POINT('',(29.8,-1.8,0.));
#16842=CARTESIAN_POINT('',(28.6,-1.8,0.));
#16843=CARTESIAN_POINT('Origin',(34.2,-1.8,0.));
#16844=CARTESIAN_POINT('',(34.2,1.8,9.2));
#16845=CARTESIAN_POINT('',(34.2,1.8,0.));
#16846=CARTESIAN_POINT('',(34.2,-1.8,9.2));
#16847=CARTESIAN_POINT('Origin',(34.2,1.8,0.));
#16848=CARTESIAN_POINT('',(29.8,1.8,9.2));
#16849=CARTESIAN_POINT('',(29.8,1.8,0.));
#16850=CARTESIAN_POINT('',(34.2,1.8,9.2));
#16851=CARTESIAN_POINT('',(28.6,1.8,0.));
#16852=CARTESIAN_POINT('Origin',(29.8,1.8,0.));
#16853=CARTESIAN_POINT('',(29.8,1.8,9.2));
#16854=CARTESIAN_POINT('Origin',(32.,0.,9.2));
#16855=CARTESIAN_POINT('Origin',(32.,0.,0.));
#16856=CARTESIAN_POINT('',(0.,0.,0.));
#16857=CARTESIAN_POINT('Origin',(32.,-0.45,7.));
#16858=CARTESIAN_POINT('',(30.9,0.45,7.));
#16859=CARTESIAN_POINT('Origin',(32.,0.45,7.));
#16860=CARTESIAN_POINT('',(30.9,-0.45,7.));
#16861=CARTESIAN_POINT('',(30.9,-0.45,7.));
#16862=CARTESIAN_POINT('Origin',(32.,-0.45,7.));
#16863=CARTESIAN_POINT('Origin',(32.,-0.45,7.));
#16864=CARTESIAN_POINT('',(30.51,0.45,7.));
#16865=CARTESIAN_POINT('Origin',(32.,0.45,7.));
#16866=CARTESIAN_POINT('',(30.51,-0.45,7.));
#16867=CARTESIAN_POINT('',(30.51,-0.45,7.));
#16868=CARTESIAN_POINT('Origin',(32.,-0.45,7.));
#16869=CARTESIAN_POINT('Origin',(32.,0.45,7.));
#16870=CARTESIAN_POINT('Origin',(32.,-0.45,7.));
#16871=CARTESIAN_POINT('',(0.,0.,0.));
#16872=CARTESIAN_POINT('Origin',(30.6564971157456,-2.2,5.65649711574556));
#16873=CARTESIAN_POINT('',(30.5936544441036,-2.1,5.4404512904656));
#16874=CARTESIAN_POINT('',(30.5936544441036,-1.8,5.4404512904656));
#16875=CARTESIAN_POINT('',(30.5936544441036,-2.2,5.4404512904656));
#16876=CARTESIAN_POINT('',(30.4404512904656,-2.1,5.59365444410359));
#16877=CARTESIAN_POINT('Origin',(30.6564971157456,-2.1,5.65649711574556));
#16878=CARTESIAN_POINT('',(30.4404512904656,-1.8,5.59365444410359));
#16879=CARTESIAN_POINT('',(30.4404512904656,-2.2,5.59365444410359));
#16880=CARTESIAN_POINT('Origin',(30.6564971157456,-1.8,5.65649711574556));
#16881=CARTESIAN_POINT('Origin',(30.6564971157456,-2.2,8.34350288425444));
#16882=CARTESIAN_POINT('',(30.4404512904656,-2.1,8.40634555589641));
#16883=CARTESIAN_POINT('',(30.4404512904656,-1.8,8.40634555589641));
#16884=CARTESIAN_POINT('',(30.4404512904656,-2.2,8.40634555589641));
#16885=CARTESIAN_POINT('',(30.5936544441036,-2.1,8.5595487095344));
#16886=CARTESIAN_POINT('Origin',(30.6564971157456,-2.1,8.34350288425444));
#16887=CARTESIAN_POINT('',(30.5936544441036,-1.8,8.5595487095344));
#16888=CARTESIAN_POINT('',(30.5936544441036,-2.2,8.5595487095344));
#16889=CARTESIAN_POINT('Origin',(30.6564971157456,-1.8,8.34350288425444));
#16890=CARTESIAN_POINT('Origin',(33.3435028842544,-2.2,8.34350288425444));
#16891=CARTESIAN_POINT('',(33.4063455558964,-2.1,8.5595487095344));
#16892=CARTESIAN_POINT('',(33.4063455558964,-1.8,8.5595487095344));
#16893=CARTESIAN_POINT('',(33.4063455558964,-2.2,8.5595487095344));
#16894=CARTESIAN_POINT('',(33.5595487095344,-2.1,8.40634555589641));
#16895=CARTESIAN_POINT('Origin',(33.3435028842544,-2.1,8.34350288425444));
#16896=CARTESIAN_POINT('',(33.5595487095344,-1.8,8.40634555589641));
#16897=CARTESIAN_POINT('',(33.5595487095344,-2.2,8.40634555589641));
#16898=CARTESIAN_POINT('Origin',(33.3435028842544,-1.8,8.34350288425444));
#16899=CARTESIAN_POINT('Origin',(33.3435028842544,-2.2,5.65649711574556));
#16900=CARTESIAN_POINT('',(33.5595487095344,-2.1,5.59365444410359));
#16901=CARTESIAN_POINT('',(33.5595487095344,-1.8,5.59365444410359));
#16902=CARTESIAN_POINT('',(33.5595487095344,-2.2,5.59365444410359));
#16903=CARTESIAN_POINT('',(33.4063455558964,-2.1,5.4404512904656));
#16904=CARTESIAN_POINT('Origin',(33.3435028842544,-2.1,5.65649711574556));
#16905=CARTESIAN_POINT('',(33.4063455558964,-1.8,5.4404512904656));
#16906=CARTESIAN_POINT('',(33.4063455558964,-2.2,5.4404512904656));
#16907=CARTESIAN_POINT('Origin',(33.3435028842544,-1.8,5.65649711574556));
#16908=CARTESIAN_POINT('Origin',(32.,-2.1,7.));
#16909=CARTESIAN_POINT('Origin',(32.,-2.1,7.));
#16910=CARTESIAN_POINT('Origin',(32.,-2.1,7.));
#16911=CARTESIAN_POINT('Origin',(32.,-2.1,7.));
#16912=CARTESIAN_POINT('Origin',(32.,-2.1,7.));
#16913=CARTESIAN_POINT('',(30.9,-2.1,7.));
#16914=CARTESIAN_POINT('Origin',(32.,-2.1,7.));
#16915=CARTESIAN_POINT('Origin',(32.,-2.1,7.));
#16916=CARTESIAN_POINT('Origin',(32.,-1.8,7.));
#16917=CARTESIAN_POINT('Origin',(32.,-2.1,7.));
#16918=CARTESIAN_POINT('Origin',(32.,-1.8,7.));
#16919=CARTESIAN_POINT('Origin',(32.,-2.1,7.));
#16920=CARTESIAN_POINT('Origin',(32.,-1.8,7.));
#16921=CARTESIAN_POINT('Origin',(32.,-2.1,7.));
#16922=CARTESIAN_POINT('Origin',(32.,-1.8,7.));
#16923=CARTESIAN_POINT('Origin',(32.,-1.8,7.));
#16924=CARTESIAN_POINT('',(30.51,-1.35,7.));
#16925=CARTESIAN_POINT('Origin',(32.,-1.35,7.));
#16926=CARTESIAN_POINT('',(30.51,-1.8,7.));
#16927=CARTESIAN_POINT('',(30.51,-1.8,7.));
#16928=CARTESIAN_POINT('Origin',(32.,-1.8,7.));
#16929=CARTESIAN_POINT('Origin',(32.,-1.35,7.));
#16930=CARTESIAN_POINT('',(30.9,-1.35,7.));
#16931=CARTESIAN_POINT('Origin',(32.,-1.35,7.));
#16932=CARTESIAN_POINT('Origin',(32.,-2.1,7.));
#16933=CARTESIAN_POINT('',(30.9,-2.1,7.));
#16934=CARTESIAN_POINT('Origin',(32.,-1.8,7.));
#16935=CARTESIAN_POINT('',(0.,0.,0.));
#16936=CARTESIAN_POINT('Origin',(30.6564971157456,1.7,5.65649711574556));
#16937=CARTESIAN_POINT('',(30.5936544441036,1.8,5.4404512904656));
#16938=CARTESIAN_POINT('',(30.5936544441036,2.1,5.4404512904656));
#16939=CARTESIAN_POINT('',(30.5936544441036,1.7,5.4404512904656));
#16940=CARTESIAN_POINT('',(30.4404512904656,1.8,5.59365444410359));
#16941=CARTESIAN_POINT('Origin',(30.6564971157456,1.8,5.65649711574556));
#16942=CARTESIAN_POINT('',(30.4404512904656,2.1,5.59365444410359));
#16943=CARTESIAN_POINT('',(30.4404512904656,1.7,5.59365444410359));
#16944=CARTESIAN_POINT('Origin',(30.6564971157456,2.1,5.65649711574556));
#16945=CARTESIAN_POINT('Origin',(30.6564971157456,1.7,8.34350288425444));
#16946=CARTESIAN_POINT('',(30.4404512904656,1.8,8.40634555589641));
#16947=CARTESIAN_POINT('',(30.4404512904656,2.1,8.40634555589641));
#16948=CARTESIAN_POINT('',(30.4404512904656,1.7,8.40634555589641));
#16949=CARTESIAN_POINT('',(30.5936544441036,1.8,8.5595487095344));
#16950=CARTESIAN_POINT('Origin',(30.6564971157456,1.8,8.34350288425444));
#16951=CARTESIAN_POINT('',(30.5936544441036,2.1,8.5595487095344));
#16952=CARTESIAN_POINT('',(30.5936544441036,1.7,8.5595487095344));
#16953=CARTESIAN_POINT('Origin',(30.6564971157456,2.1,8.34350288425444));
#16954=CARTESIAN_POINT('Origin',(33.3435028842544,1.7,8.34350288425444));
#16955=CARTESIAN_POINT('',(33.4063455558964,1.8,8.5595487095344));
#16956=CARTESIAN_POINT('',(33.4063455558964,2.1,8.5595487095344));
#16957=CARTESIAN_POINT('',(33.4063455558964,1.7,8.5595487095344));
#16958=CARTESIAN_POINT('',(33.5595487095344,1.8,8.40634555589641));
#16959=CARTESIAN_POINT('Origin',(33.3435028842544,1.8,8.34350288425444));
#16960=CARTESIAN_POINT('',(33.5595487095344,2.1,8.40634555589641));
#16961=CARTESIAN_POINT('',(33.5595487095344,1.7,8.40634555589641));
#16962=CARTESIAN_POINT('Origin',(33.3435028842544,2.1,8.34350288425444));
#16963=CARTESIAN_POINT('Origin',(33.3435028842544,1.7,5.65649711574556));
#16964=CARTESIAN_POINT('',(33.5595487095344,1.8,5.59365444410359));
#16965=CARTESIAN_POINT('',(33.5595487095344,2.1,5.59365444410359));
#16966=CARTESIAN_POINT('',(33.5595487095344,1.7,5.59365444410359));
#16967=CARTESIAN_POINT('',(33.4063455558964,1.8,5.4404512904656));
#16968=CARTESIAN_POINT('Origin',(33.3435028842544,1.8,5.65649711574556));
#16969=CARTESIAN_POINT('',(33.4063455558964,2.1,5.4404512904656));
#16970=CARTESIAN_POINT('',(33.4063455558964,1.7,5.4404512904656));
#16971=CARTESIAN_POINT('Origin',(33.3435028842544,2.1,5.65649711574556));
#16972=CARTESIAN_POINT('Origin',(32.,1.8,7.));
#16973=CARTESIAN_POINT('Origin',(32.,1.8,7.));
#16974=CARTESIAN_POINT('Origin',(32.,1.8,7.));
#16975=CARTESIAN_POINT('Origin',(32.,1.8,7.));
#16976=CARTESIAN_POINT('Origin',(32.,1.8,7.));
#16977=CARTESIAN_POINT('',(30.51,1.8,7.));
#16978=CARTESIAN_POINT('Origin',(32.,1.8,7.));
#16979=CARTESIAN_POINT('Origin',(32.,1.8,7.));
#16980=CARTESIAN_POINT('Origin',(32.,2.1,7.));
#16981=CARTESIAN_POINT('Origin',(32.,1.8,7.));
#16982=CARTESIAN_POINT('Origin',(32.,2.1,7.));
#16983=CARTESIAN_POINT('Origin',(32.,1.8,7.));
#16984=CARTESIAN_POINT('Origin',(32.,2.1,7.));
#16985=CARTESIAN_POINT('Origin',(32.,1.8,7.));
#16986=CARTESIAN_POINT('Origin',(32.,2.1,7.));
#16987=CARTESIAN_POINT('Origin',(32.,1.35,7.));
#16988=CARTESIAN_POINT('',(30.51,1.35,7.));
#16989=CARTESIAN_POINT('',(30.51,1.35,7.));
#16990=CARTESIAN_POINT('Origin',(32.,1.35,7.));
#16991=CARTESIAN_POINT('Origin',(32.,1.35,7.));
#16992=CARTESIAN_POINT('',(30.9,1.35,7.));
#16993=CARTESIAN_POINT('Origin',(32.,1.35,7.));
#16994=CARTESIAN_POINT('Origin',(32.,1.8,7.));
#16995=CARTESIAN_POINT('',(30.9,2.1,7.));
#16996=CARTESIAN_POINT('Origin',(32.,2.1,7.));
#16997=CARTESIAN_POINT('',(30.9,1.8,7.));
#16998=CARTESIAN_POINT('Origin',(32.,2.1,7.));
#16999=CARTESIAN_POINT('',(0.,0.,0.));
#17000=CARTESIAN_POINT('Origin',(32.,-3.5,6.36338022763242));
#17001=CARTESIAN_POINT('',(32.,-3.425,6.36338022763242));
#17002=CARTESIAN_POINT('',(0.,-3.425,6.36338022763242));
#17003=CARTESIAN_POINT('',(16.,-3.425,6.36338022763242));
#17004=CARTESIAN_POINT('',(32.,-2.825,6.36338022763242));
#17005=CARTESIAN_POINT('',(32.,-3.5,6.36338022763242));
#17006=CARTESIAN_POINT('',(0.,-2.825,6.36338022763242));
#17007=CARTESIAN_POINT('',(16.,-2.825,6.36338022763242));
#17008=CARTESIAN_POINT('',(0.,-3.5,6.36338022763242));
#17009=CARTESIAN_POINT('Origin',(0.,-3.5,7.63661977236758));
#17010=CARTESIAN_POINT('',(0.,-3.425,7.63661977236758));
#17011=CARTESIAN_POINT('',(32.,-3.425,7.63661977236758));
#17012=CARTESIAN_POINT('',(0.,-3.425,7.63661977236758));
#17013=CARTESIAN_POINT('',(0.,-2.825,7.63661977236758));
#17014=CARTESIAN_POINT('',(0.,-3.5,7.63661977236758));
#17015=CARTESIAN_POINT('',(32.,-2.825,7.63661977236758));
#17016=CARTESIAN_POINT('',(0.,-2.825,7.63661977236758));
#17017=CARTESIAN_POINT('',(32.,-3.5,7.63661977236758));
#17018=CARTESIAN_POINT('Origin',(0.,-3.425,7.));
#17019=CARTESIAN_POINT('',(0.,-3.425,7.73661977236758));
#17020=CARTESIAN_POINT('',(32.,-3.425,7.73661977236758));
#17021=CARTESIAN_POINT('',(0.,-3.425,7.73661977236758));
#17022=CARTESIAN_POINT('',(0.,-3.425,6.26338022763242));
#17023=CARTESIAN_POINT('Origin',(0.,-3.425,7.));
#17024=CARTESIAN_POINT('',(32.,-3.425,6.26338022763242));
#17025=CARTESIAN_POINT('',(32.,-3.425,6.26338022763242));
#17026=CARTESIAN_POINT('Origin',(32.,-3.425,7.));
#17027=CARTESIAN_POINT('Origin',(0.,-3.425,7.));
#17028=CARTESIAN_POINT('Origin',(32.,-3.425,7.));
#17029=CARTESIAN_POINT('Origin',(0.,-3.5,7.));
#17030=CARTESIAN_POINT('Origin',(0.,-2.825,7.));
#17031=CARTESIAN_POINT('Origin',(32.,-3.5,7.));
#17032=CARTESIAN_POINT('Origin',(32.,-2.825,7.));
#17033=CARTESIAN_POINT('Origin',(32.,-3.425,7.));
#17034=CARTESIAN_POINT('',(32.,-2.825,6.26338022763242));
#17035=CARTESIAN_POINT('',(32.,-3.425,6.26338022763242));
#17036=CARTESIAN_POINT('',(32.,-2.825,7.73661977236758));
#17037=CARTESIAN_POINT('Origin',(32.,-2.825,7.));
#17038=CARTESIAN_POINT('',(32.,-3.425,7.73661977236758));
#17039=CARTESIAN_POINT('Origin',(32.,-3.425,6.26338022763242));
#17040=CARTESIAN_POINT('',(0.,-2.825,6.26338022763242));
#17041=CARTESIAN_POINT('',(0.,-3.425,6.26338022763242));
#17042=CARTESIAN_POINT('',(32.,-2.825,6.26338022763242));
#17043=CARTESIAN_POINT('Origin',(0.,-3.425,7.73661977236758));
#17044=CARTESIAN_POINT('',(0.,-2.825,7.73661977236758));
#17045=CARTESIAN_POINT('',(0.,-2.825,7.73661977236758));
#17046=CARTESIAN_POINT('',(0.,-3.425,7.73661977236758));
#17047=CARTESIAN_POINT('Origin',(0.,-3.425,7.));
#17048=CARTESIAN_POINT('Origin',(0.,-2.825,7.));
#17049=CARTESIAN_POINT('Origin',(0.,-2.825,7.));
#17050=CARTESIAN_POINT('',(0.,0.,0.));
#17051=CARTESIAN_POINT('Origin',(5.8,-2.5,0.8));
#17052=CARTESIAN_POINT('',(5.5,-2.76457513110646,2.4));
#17053=CARTESIAN_POINT('',(5.5,-2.76457513110646,0.8));
#17054=CARTESIAN_POINT('',(5.5,-2.76457513110646,0.8));
#17055=CARTESIAN_POINT('',(6.1,-2.76457513110646,2.4));
#17056=CARTESIAN_POINT('Origin',(5.8,-2.5,2.4));
#17057=CARTESIAN_POINT('',(6.1,-2.76457513110646,0.8));
#17058=CARTESIAN_POINT('',(6.1,-2.76457513110646,0.8));
#17059=CARTESIAN_POINT('Origin',(5.8,-2.5,0.8));
#17060=CARTESIAN_POINT('Origin',(5.8,-2.5,0.8));
#17061=CARTESIAN_POINT('',(5.5,-2.23542486889354,0.8));
#17062=CARTESIAN_POINT('',(5.5,-2.23542486889354,2.4));
#17063=CARTESIAN_POINT('',(5.5,-2.23542486889354,0.8));
#17064=CARTESIAN_POINT('',(6.1,-2.23542486889354,0.8));
#17065=CARTESIAN_POINT('Origin',(5.8,-2.5,0.8));
#17066=CARTESIAN_POINT('',(6.1,-2.23542486889354,2.4));
#17067=CARTESIAN_POINT('',(6.1,-2.23542486889354,0.8));
#17068=CARTESIAN_POINT('Origin',(5.8,-2.5,2.4));
#17069=CARTESIAN_POINT('Origin',(5.8,-2.5,0.8));
#17070=CARTESIAN_POINT('',(5.5,0.35,0.8));
#17071=CARTESIAN_POINT('',(6.1,-2.85,0.8));
#17072=CARTESIAN_POINT('',(5.575,-2.5,0.8));
#17073=CARTESIAN_POINT('Origin',(5.8,-2.5,0.8));
#17074=CARTESIAN_POINT('Origin',(5.8,2.5,0.8));
#17075=CARTESIAN_POINT('',(5.5,2.23542486889354,2.4));
#17076=CARTESIAN_POINT('',(5.5,2.23542486889354,0.8));
#17077=CARTESIAN_POINT('',(5.5,2.23542486889354,0.8));
#17078=CARTESIAN_POINT('',(6.1,2.23542486889354,2.4));
#17079=CARTESIAN_POINT('Origin',(5.8,2.5,2.4));
#17080=CARTESIAN_POINT('',(6.1,2.23542486889354,0.8));
#17081=CARTESIAN_POINT('',(6.1,2.23542486889354,0.8));
#17082=CARTESIAN_POINT('Origin',(5.8,2.5,0.8));
#17083=CARTESIAN_POINT('Origin',(5.8,2.5,0.8));
#17084=CARTESIAN_POINT('',(5.5,2.76457513110646,0.8));
#17085=CARTESIAN_POINT('',(5.5,2.76457513110646,2.4));
#17086=CARTESIAN_POINT('',(5.5,2.76457513110646,0.8));
#17087=CARTESIAN_POINT('',(6.1,2.76457513110646,0.8));
#17088=CARTESIAN_POINT('Origin',(5.8,2.5,0.8));
#17089=CARTESIAN_POINT('',(6.1,2.76457513110646,2.4));
#17090=CARTESIAN_POINT('',(6.1,2.76457513110646,0.8));
#17091=CARTESIAN_POINT('Origin',(5.8,2.5,2.4));
#17092=CARTESIAN_POINT('Origin',(5.8,2.5,0.8));
#17093=CARTESIAN_POINT('',(5.5,2.85,0.8));
#17094=CARTESIAN_POINT('',(6.1,-0.35,0.8));
#17095=CARTESIAN_POINT('',(5.575,2.5,0.8));
#17096=CARTESIAN_POINT('Origin',(5.8,2.5,0.8));
#17097=CARTESIAN_POINT('Origin',(6.1,-3.2,0.));
#17098=CARTESIAN_POINT('',(6.1,-3.2,2.4));
#17099=CARTESIAN_POINT('',(6.1,-3.2,2.4));
#17100=CARTESIAN_POINT('',(6.1,-3.2,0.));
#17101=CARTESIAN_POINT('',(6.1,-3.2,0.));
#17102=CARTESIAN_POINT('',(6.1,-0.8,0.));
#17103=CARTESIAN_POINT('',(6.1,-3.2,0.));
#17104=CARTESIAN_POINT('',(6.1,-0.8,1.6));
#17105=CARTESIAN_POINT('',(6.1,-0.8,-0.05));
#17106=CARTESIAN_POINT('',(6.1,0.8,1.6));
#17107=CARTESIAN_POINT('',(6.1,-1.6,1.6));
#17108=CARTESIAN_POINT('',(6.1,0.8,0.));
#17109=CARTESIAN_POINT('',(6.1,0.8,-0.05));
#17110=CARTESIAN_POINT('',(6.1,3.2,0.));
#17111=CARTESIAN_POINT('',(6.1,-3.2,0.));
#17112=CARTESIAN_POINT('',(6.1,3.2,2.4));
#17113=CARTESIAN_POINT('',(6.1,3.2,0.));
#17114=CARTESIAN_POINT('',(6.1,-3.2,2.4));
#17115=CARTESIAN_POINT('',(6.1,-3.2,2.4));
#17116=CARTESIAN_POINT('Origin',(5.8,0.,2.4));
#17117=CARTESIAN_POINT('',(5.5,3.2,2.4));
#17118=CARTESIAN_POINT('',(6.1,3.2,2.4));
#17119=CARTESIAN_POINT('',(5.5,3.2,2.4));
#17120=CARTESIAN_POINT('Origin',(5.8,0.,2.4));
#17121=CARTESIAN_POINT('',(5.5,-3.2,2.4));
#17122=CARTESIAN_POINT('',(5.5,3.2,2.4));
#17123=CARTESIAN_POINT('',(5.5,-3.2,2.4));
#17124=CARTESIAN_POINT('Origin',(5.8,0.,2.4));
#17125=CARTESIAN_POINT('',(5.5,3.2,2.4));
#17126=CARTESIAN_POINT('Origin',(5.8,-2.5,-0.1));
#17127=CARTESIAN_POINT('',(5.575,-2.5,0.));
#17128=CARTESIAN_POINT('Origin',(5.8,-2.5,0.));
#17129=CARTESIAN_POINT('',(5.575,-2.5,-0.1));
#17130=CARTESIAN_POINT('Origin',(5.8,2.5,-0.1));
#17131=CARTESIAN_POINT('',(5.575,2.5,0.));
#17132=CARTESIAN_POINT('Origin',(5.8,2.5,0.));
#17133=CARTESIAN_POINT('',(5.575,2.5,-0.1));
#17134=CARTESIAN_POINT('Origin',(6.2,0.8,-0.1));
#17135=CARTESIAN_POINT('',(5.5,0.8,1.6));
#17136=CARTESIAN_POINT('',(6.2,0.8,1.6));
#17137=CARTESIAN_POINT('',(5.5,0.8,0.));
#17138=CARTESIAN_POINT('',(5.5,0.8,-0.05));
#17139=CARTESIAN_POINT('',(6.,0.8,0.));
#17140=CARTESIAN_POINT('Origin',(5.4,-0.8,-0.1));
#17141=CARTESIAN_POINT('',(5.5,-0.8,0.));
#17142=CARTESIAN_POINT('',(5.6,-0.8,0.));
#17143=CARTESIAN_POINT('',(5.5,-0.8,1.6));
#17144=CARTESIAN_POINT('',(5.5,-0.8,-0.05));
#17145=CARTESIAN_POINT('',(5.4,-0.8,1.6));
#17146=CARTESIAN_POINT('Origin',(5.8,0.,1.6));
#17147=CARTESIAN_POINT('',(5.5,1.6,1.6));
#17148=CARTESIAN_POINT('Origin',(5.5,3.2,0.));
#17149=CARTESIAN_POINT('',(5.5,3.2,0.));
#17150=CARTESIAN_POINT('',(5.5,3.2,0.));
#17151=CARTESIAN_POINT('',(5.5,3.2,0.));
#17152=CARTESIAN_POINT('',(5.5,-3.2,0.));
#17153=CARTESIAN_POINT('',(5.5,3.2,0.));
#17154=CARTESIAN_POINT('',(5.5,-3.2,0.));
#17155=CARTESIAN_POINT('Origin',(5.8,0.,0.));
#17156=CARTESIAN_POINT('',(5.5,-3.2,0.));
#17157=CARTESIAN_POINT('Origin',(5.8,0.,0.));
#17158=CARTESIAN_POINT('',(6.1,3.2,0.));
#17159=CARTESIAN_POINT('Origin',(6.1,3.2,0.));
#17160=CARTESIAN_POINT('Origin',(5.5,-3.2,0.));
#17161=CARTESIAN_POINT('',(0.,0.,0.));
#17162=CARTESIAN_POINT('Origin',(26.2,-2.5,0.8));
#17163=CARTESIAN_POINT('',(25.9,-2.76457513110646,2.4));
#17164=CARTESIAN_POINT('',(25.9,-2.76457513110646,0.8));
#17165=CARTESIAN_POINT('',(25.9,-2.76457513110646,0.8));
#17166=CARTESIAN_POINT('',(26.5,-2.76457513110646,2.4));
#17167=CARTESIAN_POINT('Origin',(26.2,-2.5,2.4));
#17168=CARTESIAN_POINT('',(26.5,-2.76457513110646,0.8));
#17169=CARTESIAN_POINT('',(26.5,-2.76457513110646,0.8));
#17170=CARTESIAN_POINT('Origin',(26.2,-2.5,0.8));
#17171=CARTESIAN_POINT('Origin',(26.2,-2.5,0.8));
#17172=CARTESIAN_POINT('',(25.9,-2.23542486889354,0.8));
#17173=CARTESIAN_POINT('',(25.9,-2.23542486889354,2.4));
#17174=CARTESIAN_POINT('',(25.9,-2.23542486889354,0.8));
#17175=CARTESIAN_POINT('',(26.5,-2.23542486889354,0.8));
#17176=CARTESIAN_POINT('Origin',(26.2,-2.5,0.8));
#17177=CARTESIAN_POINT('',(26.5,-2.23542486889354,2.4));
#17178=CARTESIAN_POINT('',(26.5,-2.23542486889354,0.8));
#17179=CARTESIAN_POINT('Origin',(26.2,-2.5,2.4));
#17180=CARTESIAN_POINT('Origin',(26.2,-2.5,0.8));
#17181=CARTESIAN_POINT('',(25.9,0.35,0.8));
#17182=CARTESIAN_POINT('',(26.5,-2.85,0.8));
#17183=CARTESIAN_POINT('',(25.975,-2.5,0.8));
#17184=CARTESIAN_POINT('Origin',(26.2,-2.5,0.8));
#17185=CARTESIAN_POINT('Origin',(26.2,2.5,0.8));
#17186=CARTESIAN_POINT('',(25.9,2.23542486889354,2.4));
#17187=CARTESIAN_POINT('',(25.9,2.23542486889354,0.8));
#17188=CARTESIAN_POINT('',(25.9,2.23542486889354,0.8));
#17189=CARTESIAN_POINT('',(26.5,2.23542486889354,2.4));
#17190=CARTESIAN_POINT('Origin',(26.2,2.5,2.4));
#17191=CARTESIAN_POINT('',(26.5,2.23542486889354,0.8));
#17192=CARTESIAN_POINT('',(26.5,2.23542486889354,0.8));
#17193=CARTESIAN_POINT('Origin',(26.2,2.5,0.8));
#17194=CARTESIAN_POINT('Origin',(26.2,2.5,0.8));
#17195=CARTESIAN_POINT('',(25.9,2.76457513110646,0.8));
#17196=CARTESIAN_POINT('',(25.9,2.76457513110646,2.4));
#17197=CARTESIAN_POINT('',(25.9,2.76457513110646,0.8));
#17198=CARTESIAN_POINT('',(26.5,2.76457513110646,0.8));
#17199=CARTESIAN_POINT('Origin',(26.2,2.5,0.8));
#17200=CARTESIAN_POINT('',(26.5,2.76457513110646,2.4));
#17201=CARTESIAN_POINT('',(26.5,2.76457513110646,0.8));
#17202=CARTESIAN_POINT('Origin',(26.2,2.5,2.4));
#17203=CARTESIAN_POINT('Origin',(26.2,2.5,0.8));
#17204=CARTESIAN_POINT('',(25.9,2.85,0.8));
#17205=CARTESIAN_POINT('',(26.5,-0.35,0.8));
#17206=CARTESIAN_POINT('',(25.975,2.5,0.8));
#17207=CARTESIAN_POINT('Origin',(26.2,2.5,0.8));
#17208=CARTESIAN_POINT('Origin',(26.5,-3.2,0.));
#17209=CARTESIAN_POINT('',(26.5,-3.2,2.4));
#17210=CARTESIAN_POINT('',(26.5,-3.2,2.4));
#17211=CARTESIAN_POINT('',(26.5,-3.2,0.));
#17212=CARTESIAN_POINT('',(26.5,-3.2,0.));
#17213=CARTESIAN_POINT('',(26.5,-0.8,0.));
#17214=CARTESIAN_POINT('',(26.5,-3.2,0.));
#17215=CARTESIAN_POINT('',(26.5,-0.8,1.6));
#17216=CARTESIAN_POINT('',(26.5,-0.8,-0.05));
#17217=CARTESIAN_POINT('',(26.5,0.8,1.6));
#17218=CARTESIAN_POINT('',(26.5,-1.6,1.6));
#17219=CARTESIAN_POINT('',(26.5,0.8,0.));
#17220=CARTESIAN_POINT('',(26.5,0.8,-0.05));
#17221=CARTESIAN_POINT('',(26.5,3.2,0.));
#17222=CARTESIAN_POINT('',(26.5,-3.2,0.));
#17223=CARTESIAN_POINT('',(26.5,3.2,2.4));
#17224=CARTESIAN_POINT('',(26.5,3.2,0.));
#17225=CARTESIAN_POINT('',(26.5,-3.2,2.4));
#17226=CARTESIAN_POINT('',(26.5,-3.2,2.4));
#17227=CARTESIAN_POINT('Origin',(26.2,0.,2.4));
#17228=CARTESIAN_POINT('',(25.9,3.2,2.4));
#17229=CARTESIAN_POINT('',(26.5,3.2,2.4));
#17230=CARTESIAN_POINT('',(25.9,3.2,2.4));
#17231=CARTESIAN_POINT('Origin',(26.2,0.,2.4));
#17232=CARTESIAN_POINT('',(25.9,-3.2,2.4));
#17233=CARTESIAN_POINT('',(25.9,3.2,2.4));
#17234=CARTESIAN_POINT('',(25.9,-3.2,2.4));
#17235=CARTESIAN_POINT('Origin',(26.2,0.,2.4));
#17236=CARTESIAN_POINT('',(25.9,3.2,2.4));
#17237=CARTESIAN_POINT('Origin',(26.2,-2.5,-0.1));
#17238=CARTESIAN_POINT('',(25.975,-2.5,0.));
#17239=CARTESIAN_POINT('Origin',(26.2,-2.5,0.));
#17240=CARTESIAN_POINT('',(25.975,-2.5,-0.1));
#17241=CARTESIAN_POINT('Origin',(26.2,2.5,-0.1));
#17242=CARTESIAN_POINT('',(25.975,2.5,0.));
#17243=CARTESIAN_POINT('Origin',(26.2,2.5,0.));
#17244=CARTESIAN_POINT('',(25.975,2.5,-0.1));
#17245=CARTESIAN_POINT('Origin',(26.6,0.8,-0.1));
#17246=CARTESIAN_POINT('',(25.9,0.8,1.6));
#17247=CARTESIAN_POINT('',(26.6,0.8,1.6));
#17248=CARTESIAN_POINT('',(25.9,0.8,0.));
#17249=CARTESIAN_POINT('',(25.9,0.8,-0.05));
#17250=CARTESIAN_POINT('',(26.4,0.8,0.));
#17251=CARTESIAN_POINT('Origin',(25.8,-0.8,-0.1));
#17252=CARTESIAN_POINT('',(25.9,-0.8,0.));
#17253=CARTESIAN_POINT('',(26.,-0.8,0.));
#17254=CARTESIAN_POINT('',(25.9,-0.8,1.6));
#17255=CARTESIAN_POINT('',(25.9,-0.8,-0.05));
#17256=CARTESIAN_POINT('',(25.8,-0.8,1.6));
#17257=CARTESIAN_POINT('Origin',(26.2,0.,1.6));
#17258=CARTESIAN_POINT('',(25.9,1.6,1.6));
#17259=CARTESIAN_POINT('Origin',(25.9,3.2,0.));
#17260=CARTESIAN_POINT('',(25.9,3.2,0.));
#17261=CARTESIAN_POINT('',(25.9,3.2,0.));
#17262=CARTESIAN_POINT('',(25.9,3.2,0.));
#17263=CARTESIAN_POINT('',(25.9,-3.2,0.));
#17264=CARTESIAN_POINT('',(25.9,3.2,0.));
#17265=CARTESIAN_POINT('',(25.9,-3.2,0.));
#17266=CARTESIAN_POINT('Origin',(26.2,0.,0.));
#17267=CARTESIAN_POINT('',(25.9,-3.2,0.));
#17268=CARTESIAN_POINT('Origin',(26.2,0.,0.));
#17269=CARTESIAN_POINT('',(26.5,3.2,0.));
#17270=CARTESIAN_POINT('Origin',(26.5,3.2,0.));
#17271=CARTESIAN_POINT('Origin',(25.9,-3.2,0.));
#17272=CARTESIAN_POINT('',(0.,0.,0.));
#17273=CARTESIAN_POINT('',(0.,0.,0.));
#17274=CARTESIAN_POINT('Origin',(0.,0.,0.));
#17275=CARTESIAN_POINT('',(-0.976185,-0.246528389340863,-1.19548183562566E-16));
#17276=CARTESIAN_POINT('',(-1.19548183562566E-16,-0.246528389340863,0.976185));
#17277=CARTESIAN_POINT('Origin',(0.,-0.246528389340863,0.));
#17278=CARTESIAN_POINT('Origin',(0.,-0.246528389340863,0.));
#17279=CARTESIAN_POINT('',(-1.19548183562566E-16,0.246528389340863,0.976185));
#17280=CARTESIAN_POINT('Origin',(-1.22464679914735E-16,0.,1.));
#17281=CARTESIAN_POINT('',(-0.976185,0.246528389340863,1.19548183562566E-16));
#17282=CARTESIAN_POINT('Origin',(0.,0.246528389340863,0.));
#17283=CARTESIAN_POINT('Origin',(0.,0.246528389340863,0.));
#17284=CARTESIAN_POINT('Origin',(0.,0.,0.));
#17285=CARTESIAN_POINT('',(-0.976185,0.45,-1.19548183562566E-16));
#17286=CARTESIAN_POINT('',(-0.976185,0.,-1.19548183562566E-16));
#17287=CARTESIAN_POINT('Origin',(0.,0.45,0.));
#17288=CARTESIAN_POINT('Origin',(0.,0.,0.));
#17289=CARTESIAN_POINT('',(-0.5,-0.39,-6.12323399573677E-17));
#17290=CARTESIAN_POINT('Origin',(0.,-0.39,0.));
#17291=CARTESIAN_POINT('',(-0.5,0.39,-6.12323399573677E-17));
#17292=CARTESIAN_POINT('',(-0.5,0.,-6.12323399573677E-17));
#17293=CARTESIAN_POINT('Origin',(0.,0.39,0.));
#17294=CARTESIAN_POINT('Origin',(0.,0.42,0.));
#17295=CARTESIAN_POINT('',(-0.56,0.45,-6.85802207522518E-17));
#17296=CARTESIAN_POINT('',(-0.53,0.42,-6.49062803548097E-17));
#17297=CARTESIAN_POINT('Origin',(0.,0.45,0.));
#17298=CARTESIAN_POINT('Origin',(0.976185,0.45,0.));
#17299=CARTESIAN_POINT('Origin',(0.,0.,0.));
#17300=CARTESIAN_POINT('',(-0.976185,-0.45,-1.19548183562566E-16));
#17301=CARTESIAN_POINT('Origin',(0.,-0.45,0.));
#17302=CARTESIAN_POINT('',(-0.976185,0.,-1.19548183562566E-16));
#17303=CARTESIAN_POINT('Origin',(0.56,-0.45,0.));
#17304=CARTESIAN_POINT('',(-0.56,-0.45,-6.85802207522518E-17));
#17305=CARTESIAN_POINT('Origin',(0.,-0.45,0.));
#17306=CARTESIAN_POINT('Origin',(0.,-0.42,0.));
#17307=CARTESIAN_POINT('',(-0.53,-0.42,-6.49062803548097E-17));
#17308=CARTESIAN_POINT('',(0.,0.,0.));
#17309=CARTESIAN_POINT('Origin',(0.,0.,0.));
#17310=CARTESIAN_POINT('',(-1.023815,0.246528389340863,-1.25381176266905E-16));
#17311=CARTESIAN_POINT('',(-1.25381176266905E-16,0.246528389340863,1.023815));
#17312=CARTESIAN_POINT('Origin',(0.,0.246528389340863,0.));
#17313=CARTESIAN_POINT('Origin',(0.,0.246528389340863,0.));
#17314=CARTESIAN_POINT('',(-1.25381176266905E-16,-0.246528389340863,1.023815));
#17315=CARTESIAN_POINT('Origin',(-1.22464679914735E-16,0.,1.));
#17316=CARTESIAN_POINT('',(-1.023815,-0.246528389340863,1.25381176266905E-16));
#17317=CARTESIAN_POINT('Origin',(0.,-0.246528389340863,0.));
#17318=CARTESIAN_POINT('Origin',(0.,-0.246528389340863,0.));
#17319=CARTESIAN_POINT('Origin',(0.,0.,0.));
#17320=CARTESIAN_POINT('',(-1.023815,-0.45,-1.25381176266905E-16));
#17321=CARTESIAN_POINT('Origin',(0.,-0.45,0.));
#17322=CARTESIAN_POINT('',(-1.023815,0.,-1.25381176266905E-16));
#17323=CARTESIAN_POINT('Origin',(1.44,0.45,0.));
#17324=CARTESIAN_POINT('',(-1.44,0.45,-1.76349139077219E-16));
#17325=CARTESIAN_POINT('Origin',(0.,0.45,0.));
#17326=CARTESIAN_POINT('',(-1.023815,0.45,-1.25381176266905E-16));
#17327=CARTESIAN_POINT('Origin',(0.,0.45,0.));
#17328=CARTESIAN_POINT('Origin',(0.,0.42,0.));
#17329=CARTESIAN_POINT('',(-1.5,0.39,-1.83697019872103E-16));
#17330=CARTESIAN_POINT('Origin',(0.,0.39,0.));
#17331=CARTESIAN_POINT('',(-1.47,0.42,-1.80023079474661E-16));
#17332=CARTESIAN_POINT('Origin',(0.,0.,0.));
#17333=CARTESIAN_POINT('',(-1.5,-0.39,-1.83697019872103E-16));
#17334=CARTESIAN_POINT('Origin',(0.,-0.39,0.));
#17335=CARTESIAN_POINT('',(-1.5,0.,-1.83697019872103E-16));
#17336=CARTESIAN_POINT('Origin',(0.,-0.42,0.));
#17337=CARTESIAN_POINT('',(-1.44,-0.45,-1.76349139077219E-16));
#17338=CARTESIAN_POINT('Origin',(0.,-0.45,0.));
#17339=CARTESIAN_POINT('',(-1.47,-0.42,-1.80023079474661E-16));
#17340=CARTESIAN_POINT('Origin',(1.023815,-0.45,0.));
#17341=CARTESIAN_POINT('Origin',(0.,0.,0.));
#17342=CARTESIAN_POINT('',(-1.023815,0.,-1.25381176266905E-16));
#17343=CARTESIAN_POINT('',(0.,0.,0.));
#17344=CARTESIAN_POINT('Origin',(1.,0.,0.));
#17345=CARTESIAN_POINT('',(1.,-1.78583896120461E-33,0.23815));
#17346=CARTESIAN_POINT('',(1.,-1.78583896120461E-33,-0.23815));
#17347=CARTESIAN_POINT('Origin',(1.,0.,0.));
#17348=CARTESIAN_POINT('Origin',(0.707106781186548,0.,-0.707106781186547));
#17349=CARTESIAN_POINT('',(0.875504261126124,-1.78583896120461E-33,-0.538709301246971));
#17350=CARTESIAN_POINT('',(0.538709301246971,-1.78583896120461E-33,-0.875504261126124));
#17351=CARTESIAN_POINT('Origin',(0.707106781186548,0.,-0.707106781186547));
#17352=CARTESIAN_POINT('Origin',(6.12323399573677E-17,0.,-1.));
#17353=CARTESIAN_POINT('',(0.23815,-1.78583896120461E-33,-1.));
#17354=CARTESIAN_POINT('',(-0.23815,-1.78583896120461E-33,-1.));
#17355=CARTESIAN_POINT('Origin',(6.12323399573677E-17,0.,-1.));
#17356=CARTESIAN_POINT('Origin',(-0.707106781186547,0.,-0.707106781186548));
#17357=CARTESIAN_POINT('',(-0.538709301246971,-1.78583896120461E-33,-0.875504261126124));
#17358=CARTESIAN_POINT('',(-0.875504261126124,-1.78583896120461E-33,-0.538709301246971));
#17359=CARTESIAN_POINT('Origin',(-0.707106781186547,0.,-0.707106781186548));
#17360=CARTESIAN_POINT('Origin',(-1.,0.,-1.22464679914735E-16));
#17361=CARTESIAN_POINT('',(-1.,-1.78583896120461E-33,-0.23815));
#17362=CARTESIAN_POINT('',(-1.,-1.78583896120461E-33,0.23815));
#17363=CARTESIAN_POINT('Origin',(-1.,0.,-1.22464679914735E-16));
#17364=CARTESIAN_POINT('Origin',(-0.707106781186548,0.,0.707106781186547));
#17365=CARTESIAN_POINT('',(-0.875504261126124,-7.94881478324376E-33,0.538709301246971));
#17366=CARTESIAN_POINT('',(-0.538709301246971,4.37713686083455E-33,0.875504261126124));
#17367=CARTESIAN_POINT('Origin',(-0.707106781186548,0.,0.707106781186547));
#17368=CARTESIAN_POINT('Origin',(-1.83697019872103E-16,0.,1.));
#17369=CARTESIAN_POINT('',(-0.23815,-1.78583896120461E-33,1.));
#17370=CARTESIAN_POINT('',(0.23815,-1.78583896120461E-33,1.));
#17371=CARTESIAN_POINT('Origin',(-1.83697019872103E-16,0.,1.));
#17372=CARTESIAN_POINT('Origin',(0.707106781186547,0.,0.707106781186548));
#17373=CARTESIAN_POINT('',(0.538709301246971,-4.86732687222419E-33,0.875504261126124));
#17374=CARTESIAN_POINT('',(0.875504261126124,1.29564894981497E-33,0.538709301246971));
#17375=CARTESIAN_POINT('Origin',(0.707106781186547,0.,0.707106781186548));
#17376=CARTESIAN_POINT('',(0.,0.,0.));
#17377=CARTESIAN_POINT('Origin',(0.707106781186547,0.,0.707106781186548));
#17378=CARTESIAN_POINT('',(0.504455939115715,-0.04763,0.841298510752802));
#17379=CARTESIAN_POINT('',(0.841298510752802,-0.04763,0.504455939115715));
#17380=CARTESIAN_POINT('Ctrl Pts',(0.504455939115715,-0.04763,0.841298510752802));
#17381=CARTESIAN_POINT('Ctrl Pts',(0.508899795931835,-0.0740444353928835,
0.838633903678357));
#17382=CARTESIAN_POINT('Ctrl Pts',(0.517157748491652,-0.0999305678883309,
0.833661031856294));
#17383=CARTESIAN_POINT('Ctrl Pts',(0.537715343527944,-0.142345102874864,
0.820511285096538));
#17384=CARTESIAN_POINT('Ctrl Pts',(0.548874290046456,-0.159766064500479,
0.813159949759));
#17385=CARTESIAN_POINT('Ctrl Pts',(0.573915184558107,-0.190326085855194,
0.795684265985089));
#17386=CARTESIAN_POINT('Ctrl Pts',(0.587792702767295,-0.203463743702801,
0.78555112003688));
#17387=CARTESIAN_POINT('Ctrl Pts',(0.615966552324775,-0.224161999508995,
0.763642258217233));
#17388=CARTESIAN_POINT('Ctrl Pts',(0.631684198665438,-0.232861760990032,
0.750785745543687));
#17389=CARTESIAN_POINT('Ctrl Pts',(0.663382628119203,-0.244251601209411,
0.722929908501543));
#17390=CARTESIAN_POINT('Ctrl Pts',(0.679352081686668,-0.246942143572133,
0.707917883896095));
#17391=CARTESIAN_POINT('Ctrl Pts',(0.707917883896095,-0.246942143572133,
0.679352081686668));
#17392=CARTESIAN_POINT('Ctrl Pts',(0.722929908501543,-0.244251601209411,
0.663382628119203));
#17393=CARTESIAN_POINT('Ctrl Pts',(0.750785745543687,-0.232861760990032,
0.631684198665439));
#17394=CARTESIAN_POINT('Ctrl Pts',(0.763642258217232,-0.224161999508995,
0.615966552324775));
#17395=CARTESIAN_POINT('Ctrl Pts',(0.78555112003688,-0.203463743702801,
0.587792702767295));
#17396=CARTESIAN_POINT('Ctrl Pts',(0.795684265985088,-0.190326085855194,
0.573915184558108));
#17397=CARTESIAN_POINT('Ctrl Pts',(0.813159949759,-0.15976606450048,0.548874290046456));
#17398=CARTESIAN_POINT('Ctrl Pts',(0.820511285096538,-0.142345102874864,
0.537715343527944));
#17399=CARTESIAN_POINT('Ctrl Pts',(0.833661031856294,-0.099930567888331,
0.517157748491653));
#17400=CARTESIAN_POINT('Ctrl Pts',(0.838633903678357,-0.0740444353928835,
0.508899795931835));
#17401=CARTESIAN_POINT('Ctrl Pts',(0.841298510752801,-0.0476299999999999,
0.504455939115715));
#17402=CARTESIAN_POINT('',(0.528110872004958,-0.04763,0.871530771444223));
#17403=CARTESIAN_POINT('Origin',(0.707106781186547,-0.04763,0.707106781186548));
#17404=CARTESIAN_POINT('',(0.871530771444223,-0.04763,0.528110872004959));
#17405=CARTESIAN_POINT('Ctrl Pts',(0.871530771444223,-0.0476300000000001,
0.528110872004958));
#17406=CARTESIAN_POINT('Ctrl Pts',(0.87014664509073,-0.0609922781173483,
0.530395067942936));
#17407=CARTESIAN_POINT('Ctrl Pts',(0.868149331745851,-0.0742967091364493,
0.533674141594226));
#17408=CARTESIAN_POINT('Ctrl Pts',(0.85981294420286,-0.115492077056649,
0.54708917182331));
#17409=CARTESIAN_POINT('Ctrl Pts',(0.850993704737257,-0.141695629206859,
0.560922177770136));
#17410=CARTESIAN_POINT('Ctrl Pts',(0.830754510485543,-0.181890537957859,
0.590422647829571));
#17411=CARTESIAN_POINT('Ctrl Pts',(0.816896541396381,-0.201072148666545,
0.609616703125488));
#17412=CARTESIAN_POINT('Ctrl Pts',(0.792310597819928,-0.223955109275652,
0.641117951819998));
#17413=CARTESIAN_POINT('Ctrl Pts',(0.779109323683612,-0.232742381310829,
0.657208095763053));
#17414=CARTESIAN_POINT('Ctrl Pts',(0.750552691816206,-0.244234834628584,
0.68964083160521));
#17415=CARTESIAN_POINT('Ctrl Pts',(0.735185187071673,-0.246942143572133,
0.705971972091755));
#17416=CARTESIAN_POINT('Ctrl Pts',(0.705971972091754,-0.246942143572133,
0.735185187071673));
#17417=CARTESIAN_POINT('Ctrl Pts',(0.689640831605209,-0.244234834628584,
0.750552691816206));
#17418=CARTESIAN_POINT('Ctrl Pts',(0.657208095763052,-0.232742381310829,
0.779109323683612));
#17419=CARTESIAN_POINT('Ctrl Pts',(0.641117951819998,-0.223955109275652,
0.792310597819928));
#17420=CARTESIAN_POINT('Ctrl Pts',(0.609616703125487,-0.201072148666545,
0.816896541396382));
#17421=CARTESIAN_POINT('Ctrl Pts',(0.590422647829571,-0.181890537957858,
0.830754510485544));
#17422=CARTESIAN_POINT('Ctrl Pts',(0.560922177770135,-0.141695629206858,
0.850993704737257));
#17423=CARTESIAN_POINT('Ctrl Pts',(0.547089171823309,-0.115492077056649,
0.859812944202861));
#17424=CARTESIAN_POINT('Ctrl Pts',(0.533674141594226,-0.0742967091364491,
0.868149331745852));
#17425=CARTESIAN_POINT('Ctrl Pts',(0.530395067942936,-0.0609922781173483,
0.870146645090731));
#17426=CARTESIAN_POINT('Ctrl Pts',(0.528110872004958,-0.0476300000000001,
0.871530771444223));
#17427=CARTESIAN_POINT('Origin',(0.707106781186547,-0.04763,0.707106781186548));
#17428=CARTESIAN_POINT('Origin',(0.,-0.166705,0.));
#17429=CARTESIAN_POINT('',(0.242834539687906,-0.04763,0.989696097314));
#17430=CARTESIAN_POINT('Origin',(0.,-0.04763,0.));
#17431=CARTESIAN_POINT('',(-0.242834539687907,-0.04763,0.989696097314));
#17432=CARTESIAN_POINT('Ctrl Pts',(0.242834539687906,-0.04763,0.989696097314));
#17433=CARTESIAN_POINT('Ctrl Pts',(0.24024064412003,-0.0609922781173483,
0.990332542620729));
#17434=CARTESIAN_POINT('Ctrl Pts',(0.236509675094874,-0.0742967091364492,
0.991238884025248));
#17435=CARTESIAN_POINT('Ctrl Pts',(0.221129100087819,-0.115492077056649,
0.994830026707808));
#17436=CARTESIAN_POINT('Ctrl Pts',(0.205111543747588,-0.141695629206859,
0.998375294985966));
#17437=CARTESIAN_POINT('Ctrl Pts',(0.169940289819232,-0.181890537957859,
1.00492400591205));
#17438=CARTESIAN_POINT('Ctrl Pts',(0.1465689792446,-0.201072148666545,1.00869718865384));
#17439=CARTESIAN_POINT('Ctrl Pts',(0.106909345252087,-0.223955109275652,
1.01358704779679));
#17440=CARTESIAN_POINT('Ctrl Pts',(0.0861971848975941,-0.232742381310829,
1.0156297872271));
#17441=CARTESIAN_POINT('Ctrl Pts',(0.0430711894098822,-0.244234834628584,
1.01837060663223));
#17442=CARTESIAN_POINT('Ctrl Pts',(0.0206568624125605,-0.246942143572133,
1.019052));
#17443=CARTESIAN_POINT('Ctrl Pts',(-0.0206568624125608,-0.246942143572133,
1.019052));
#17444=CARTESIAN_POINT('Ctrl Pts',(-0.0430711894098825,-0.244234834628584,
1.01837060663223));
#17445=CARTESIAN_POINT('Ctrl Pts',(-0.0861971848975943,-0.232742381310829,
1.0156297872271));
#17446=CARTESIAN_POINT('Ctrl Pts',(-0.106909345252088,-0.223955109275652,
1.01358704779679));
#17447=CARTESIAN_POINT('Ctrl Pts',(-0.1465689792446,-0.201072148666545,
1.00869718865384));
#17448=CARTESIAN_POINT('Ctrl Pts',(-0.169940289819232,-0.181890537957859,
1.00492400591205));
#17449=CARTESIAN_POINT('Ctrl Pts',(-0.205111543747588,-0.141695629206859,
0.998375294985966));
#17450=CARTESIAN_POINT('Ctrl Pts',(-0.221129100087819,-0.115492077056649,
0.994830026707808));
#17451=CARTESIAN_POINT('Ctrl Pts',(-0.236509675094875,-0.0742967091364493,
0.991238884025248));
#17452=CARTESIAN_POINT('Ctrl Pts',(-0.24024064412003,-0.0609922781173483,
0.990332542620729));
#17453=CARTESIAN_POINT('Ctrl Pts',(-0.242834539687907,-0.04763,0.989696097314));
#17454=CARTESIAN_POINT('',(-0.528110872004959,-0.04763,0.871530771444223));
#17455=CARTESIAN_POINT('Origin',(0.,-0.04763,0.));
#17456=CARTESIAN_POINT('',(-0.871530771444223,-0.04763,0.528110872004958));
#17457=CARTESIAN_POINT('Ctrl Pts',(-0.528110872004958,-0.0476300000000001,
0.871530771444223));
#17458=CARTESIAN_POINT('Ctrl Pts',(-0.530395067942936,-0.0609922781173484,
0.87014664509073));
#17459=CARTESIAN_POINT('Ctrl Pts',(-0.533674141594226,-0.0742967091364493,
0.868149331745851));
#17460=CARTESIAN_POINT('Ctrl Pts',(-0.54708917182331,-0.115492077056649,
0.85981294420286));
#17461=CARTESIAN_POINT('Ctrl Pts',(-0.560922177770136,-0.141695629206859,
0.850993704737257));
#17462=CARTESIAN_POINT('Ctrl Pts',(-0.590422647829571,-0.181890537957859,
0.830754510485543));
#17463=CARTESIAN_POINT('Ctrl Pts',(-0.609616703125488,-0.201072148666545,
0.816896541396381));
#17464=CARTESIAN_POINT('Ctrl Pts',(-0.641117951819998,-0.223955109275652,
0.792310597819928));
#17465=CARTESIAN_POINT('Ctrl Pts',(-0.657208095763053,-0.232742381310829,
0.779109323683611));
#17466=CARTESIAN_POINT('Ctrl Pts',(-0.68964083160521,-0.244234834628584,
0.750552691816205));
#17467=CARTESIAN_POINT('Ctrl Pts',(-0.705971972091755,-0.246942143572133,
0.735185187071673));
#17468=CARTESIAN_POINT('Ctrl Pts',(-0.735185187071673,-0.246942143572133,
0.705971972091754));
#17469=CARTESIAN_POINT('Ctrl Pts',(-0.750552691816206,-0.244234834628584,
0.689640831605209));
#17470=CARTESIAN_POINT('Ctrl Pts',(-0.779109323683612,-0.232742381310829,
0.657208095763052));
#17471=CARTESIAN_POINT('Ctrl Pts',(-0.792310597819928,-0.223955109275652,
0.641117951819998));
#17472=CARTESIAN_POINT('Ctrl Pts',(-0.816896541396382,-0.201072148666545,
0.609616703125487));
#17473=CARTESIAN_POINT('Ctrl Pts',(-0.830754510485544,-0.181890537957858,
0.590422647829571));
#17474=CARTESIAN_POINT('Ctrl Pts',(-0.850993704737257,-0.141695629206858,
0.560922177770135));
#17475=CARTESIAN_POINT('Ctrl Pts',(-0.859812944202861,-0.115492077056649,
0.547089171823309));
#17476=CARTESIAN_POINT('Ctrl Pts',(-0.868149331745852,-0.0742967091364491,
0.533674141594226));
#17477=CARTESIAN_POINT('Ctrl Pts',(-0.870146645090731,-0.0609922781173483,
0.530395067942936));
#17478=CARTESIAN_POINT('Ctrl Pts',(-0.871530771444223,-0.04763,0.528110872004958));
#17479=CARTESIAN_POINT('',(-0.989696097314,-0.04763,0.242834539687906));
#17480=CARTESIAN_POINT('Origin',(0.,-0.04763,0.));
#17481=CARTESIAN_POINT('',(-1.019052,-0.246942143572133,1.248489836334E-16));
#17482=CARTESIAN_POINT('Ctrl Pts',(-0.989696097314,-0.04763,0.242834539687906));
#17483=CARTESIAN_POINT('Ctrl Pts',(-0.990332542620729,-0.0609922781173483,
0.24024064412003));
#17484=CARTESIAN_POINT('Ctrl Pts',(-0.991238884025248,-0.0742967091364492,
0.236509675094874));
#17485=CARTESIAN_POINT('Ctrl Pts',(-0.994830026707808,-0.115492077056649,
0.221129100087819));
#17486=CARTESIAN_POINT('Ctrl Pts',(-0.998375294985966,-0.141695629206859,
0.205111543747588));
#17487=CARTESIAN_POINT('Ctrl Pts',(-1.00492400591205,-0.181890537957859,
0.169940289819232));
#17488=CARTESIAN_POINT('Ctrl Pts',(-1.00869718865384,-0.201072148666545,
0.1465689792446));
#17489=CARTESIAN_POINT('Ctrl Pts',(-1.01358704779679,-0.223955109275652,
0.106909345252088));
#17490=CARTESIAN_POINT('Ctrl Pts',(-1.0156297872271,-0.232742381310829,
0.0861971848975944));
#17491=CARTESIAN_POINT('Ctrl Pts',(-1.01837060663223,-0.244234834628584,
0.0430711894098825));
#17492=CARTESIAN_POINT('Ctrl Pts',(-1.019052,-0.246942143572133,0.0206568624125608));
#17493=CARTESIAN_POINT('Ctrl Pts',(-1.019052,-0.246942143572133,1.2490009027033E-16));
#17494=CARTESIAN_POINT('',(-1.019052,-0.28578,1.24797876996471E-16));
#17495=CARTESIAN_POINT('',(-1.019052,-0.166705,1.24797876996471E-16));
#17496=CARTESIAN_POINT('Origin',(0.,-0.28578,0.));
#17497=CARTESIAN_POINT('',(-0.989696097314,-0.04763,-0.242834539687906));
#17498=CARTESIAN_POINT('Ctrl Pts',(-1.019052,-0.246942143572133,1.2490009027033E-16));
#17499=CARTESIAN_POINT('Ctrl Pts',(-1.019052,-0.246942143572133,-0.0206568624125605));
#17500=CARTESIAN_POINT('Ctrl Pts',(-1.01837060663223,-0.244234834628584,
-0.0430711894098822));
#17501=CARTESIAN_POINT('Ctrl Pts',(-1.0156297872271,-0.232742381310829,
-0.0861971848975941));
#17502=CARTESIAN_POINT('Ctrl Pts',(-1.01358704779679,-0.223955109275652,
-0.106909345252087));
#17503=CARTESIAN_POINT('Ctrl Pts',(-1.00869718865384,-0.201072148666546,
-0.1465689792446));
#17504=CARTESIAN_POINT('Ctrl Pts',(-1.00492400591205,-0.181890537957859,
-0.169940289819232));
#17505=CARTESIAN_POINT('Ctrl Pts',(-0.998375294985966,-0.141695629206859,
-0.205111543747588));
#17506=CARTESIAN_POINT('Ctrl Pts',(-0.994830026707808,-0.11549207705665,
-0.221129100087819));
#17507=CARTESIAN_POINT('Ctrl Pts',(-0.991238884025248,-0.0742967091364495,
-0.236509675094874));
#17508=CARTESIAN_POINT('Ctrl Pts',(-0.990332542620729,-0.0609922781173484,
-0.24024064412003));
#17509=CARTESIAN_POINT('Ctrl Pts',(-0.989696097314,-0.0476300000000001,
-0.242834539687907));
#17510=CARTESIAN_POINT('',(-0.871530771444223,-0.04763,-0.528110872004958));
#17511=CARTESIAN_POINT('Origin',(0.,-0.04763,0.));
#17512=CARTESIAN_POINT('',(-0.528110872004958,-0.04763,-0.871530771444223));
#17513=CARTESIAN_POINT('Ctrl Pts',(-0.871530771444223,-0.0476300000000001,
-0.528110872004958));
#17514=CARTESIAN_POINT('Ctrl Pts',(-0.87014664509073,-0.0609922781173484,
-0.530395067942936));
#17515=CARTESIAN_POINT('Ctrl Pts',(-0.868149331745851,-0.0742967091364494,
-0.533674141594226));
#17516=CARTESIAN_POINT('Ctrl Pts',(-0.85981294420286,-0.115492077056649,
-0.54708917182331));
#17517=CARTESIAN_POINT('Ctrl Pts',(-0.850993704737257,-0.141695629206859,
-0.560922177770136));
#17518=CARTESIAN_POINT('Ctrl Pts',(-0.830754510485543,-0.181890537957859,
-0.590422647829571));
#17519=CARTESIAN_POINT('Ctrl Pts',(-0.816896541396381,-0.201072148666546,
-0.609616703125488));
#17520=CARTESIAN_POINT('Ctrl Pts',(-0.792310597819928,-0.223955109275652,
-0.641117951819999));
#17521=CARTESIAN_POINT('Ctrl Pts',(-0.779109323683611,-0.232742381310829,
-0.657208095763053));
#17522=CARTESIAN_POINT('Ctrl Pts',(-0.750552691816205,-0.244234834628584,
-0.68964083160521));
#17523=CARTESIAN_POINT('Ctrl Pts',(-0.735185187071673,-0.246942143572133,
-0.705971972091755));
#17524=CARTESIAN_POINT('Ctrl Pts',(-0.705971972091754,-0.246942143572133,
-0.735185187071673));
#17525=CARTESIAN_POINT('Ctrl Pts',(-0.68964083160521,-0.244234834628584,
-0.750552691816206));
#17526=CARTESIAN_POINT('Ctrl Pts',(-0.657208095763052,-0.232742381310829,
-0.779109323683612));
#17527=CARTESIAN_POINT('Ctrl Pts',(-0.641117951819998,-0.223955109275652,
-0.792310597819928));
#17528=CARTESIAN_POINT('Ctrl Pts',(-0.609616703125488,-0.201072148666545,
-0.816896541396381));
#17529=CARTESIAN_POINT('Ctrl Pts',(-0.590422647829571,-0.181890537957859,
-0.830754510485543));
#17530=CARTESIAN_POINT('Ctrl Pts',(-0.560922177770136,-0.141695629206859,
-0.850993704737257));
#17531=CARTESIAN_POINT('Ctrl Pts',(-0.54708917182331,-0.115492077056649,
-0.85981294420286));
#17532=CARTESIAN_POINT('Ctrl Pts',(-0.533674141594226,-0.0742967091364494,
-0.868149331745852));
#17533=CARTESIAN_POINT('Ctrl Pts',(-0.530395067942936,-0.0609922781173484,
-0.870146645090731));
#17534=CARTESIAN_POINT('Ctrl Pts',(-0.528110872004958,-0.0476300000000001,
-0.871530771444223));
#17535=CARTESIAN_POINT('',(-0.242834539687906,-0.04763,-0.989696097314));
#17536=CARTESIAN_POINT('Origin',(0.,-0.04763,0.));
#17537=CARTESIAN_POINT('',(0.242834539687906,-0.04763,-0.989696097314));
#17538=CARTESIAN_POINT('Ctrl Pts',(-0.242834539687907,-0.04763,-0.989696097314));
#17539=CARTESIAN_POINT('Ctrl Pts',(-0.24024064412003,-0.0609922781173483,
-0.990332542620729));
#17540=CARTESIAN_POINT('Ctrl Pts',(-0.236509675094874,-0.0742967091364493,
-0.991238884025248));
#17541=CARTESIAN_POINT('Ctrl Pts',(-0.221129100087819,-0.115492077056649,
-0.994830026707808));
#17542=CARTESIAN_POINT('Ctrl Pts',(-0.205111543747588,-0.141695629206859,
-0.998375294985966));
#17543=CARTESIAN_POINT('Ctrl Pts',(-0.169940289819232,-0.181890537957859,
-1.00492400591205));
#17544=CARTESIAN_POINT('Ctrl Pts',(-0.1465689792446,-0.201072148666545,
-1.00869718865384));
#17545=CARTESIAN_POINT('Ctrl Pts',(-0.106909345252087,-0.223955109275652,
-1.01358704779679));
#17546=CARTESIAN_POINT('Ctrl Pts',(-0.0861971848975942,-0.232742381310829,
-1.0156297872271));
#17547=CARTESIAN_POINT('Ctrl Pts',(-0.0430711894098823,-0.244234834628584,
-1.01837060663223));
#17548=CARTESIAN_POINT('Ctrl Pts',(-0.0206568624125606,-0.246942143572133,
-1.019052));
#17549=CARTESIAN_POINT('Ctrl Pts',(0.0206568624125607,-0.246942143572133,
-1.019052));
#17550=CARTESIAN_POINT('Ctrl Pts',(0.0430711894098824,-0.244234834628584,
-1.01837060663223));
#17551=CARTESIAN_POINT('Ctrl Pts',(0.0861971848975943,-0.232742381310829,
-1.0156297872271));
#17552=CARTESIAN_POINT('Ctrl Pts',(0.106909345252088,-0.223955109275652,
-1.01358704779679));
#17553=CARTESIAN_POINT('Ctrl Pts',(0.1465689792446,-0.201072148666545,-1.00869718865384));
#17554=CARTESIAN_POINT('Ctrl Pts',(0.169940289819232,-0.181890537957859,
-1.00492400591205));
#17555=CARTESIAN_POINT('Ctrl Pts',(0.205111543747588,-0.141695629206859,
-0.998375294985966));
#17556=CARTESIAN_POINT('Ctrl Pts',(0.221129100087819,-0.115492077056649,
-0.994830026707808));
#17557=CARTESIAN_POINT('Ctrl Pts',(0.236509675094874,-0.0742967091364493,
-0.991238884025248));
#17558=CARTESIAN_POINT('Ctrl Pts',(0.24024064412003,-0.0609922781173484,
-0.990332542620729));
#17559=CARTESIAN_POINT('Ctrl Pts',(0.242834539687907,-0.04763,-0.989696097314));
#17560=CARTESIAN_POINT('',(0.528110872004958,-0.04763,-0.871530771444223));
#17561=CARTESIAN_POINT('Origin',(0.,-0.04763,0.));
#17562=CARTESIAN_POINT('',(0.871530771444223,-0.04763,-0.528110872004958));
#17563=CARTESIAN_POINT('Ctrl Pts',(0.528110872004958,-0.0476300000000001,
-0.871530771444223));
#17564=CARTESIAN_POINT('Ctrl Pts',(0.530395067942936,-0.0609922781173484,
-0.870146645090731));
#17565=CARTESIAN_POINT('Ctrl Pts',(0.533674141594226,-0.0742967091364493,
-0.868149331745851));
#17566=CARTESIAN_POINT('Ctrl Pts',(0.54708917182331,-0.115492077056649,
-0.85981294420286));
#17567=CARTESIAN_POINT('Ctrl Pts',(0.560922177770136,-0.141695629206859,
-0.850993704737257));
#17568=CARTESIAN_POINT('Ctrl Pts',(0.590422647829571,-0.181890537957859,
-0.830754510485543));
#17569=CARTESIAN_POINT('Ctrl Pts',(0.609616703125488,-0.201072148666545,
-0.816896541396381));
#17570=CARTESIAN_POINT('Ctrl Pts',(0.641117951819998,-0.223955109275652,
-0.792310597819928));
#17571=CARTESIAN_POINT('Ctrl Pts',(0.657208095763053,-0.232742381310829,
-0.779109323683612));
#17572=CARTESIAN_POINT('Ctrl Pts',(0.68964083160521,-0.244234834628584,
-0.750552691816206));
#17573=CARTESIAN_POINT('Ctrl Pts',(0.705971972091755,-0.246942143572133,
-0.735185187071673));
#17574=CARTESIAN_POINT('Ctrl Pts',(0.735185187071673,-0.246942143572133,
-0.705971972091754));
#17575=CARTESIAN_POINT('Ctrl Pts',(0.750552691816206,-0.244234834628584,
-0.68964083160521));
#17576=CARTESIAN_POINT('Ctrl Pts',(0.779109323683612,-0.232742381310829,
-0.657208095763053));
#17577=CARTESIAN_POINT('Ctrl Pts',(0.792310597819928,-0.223955109275652,
-0.641117951819998));
#17578=CARTESIAN_POINT('Ctrl Pts',(0.816896541396381,-0.201072148666545,
-0.609616703125488));
#17579=CARTESIAN_POINT('Ctrl Pts',(0.830754510485543,-0.181890537957859,
-0.590422647829571));
#17580=CARTESIAN_POINT('Ctrl Pts',(0.850993704737257,-0.141695629206859,
-0.560922177770136));
#17581=CARTESIAN_POINT('Ctrl Pts',(0.85981294420286,-0.115492077056649,
-0.54708917182331));
#17582=CARTESIAN_POINT('Ctrl Pts',(0.868149331745851,-0.0742967091364493,
-0.533674141594226));
#17583=CARTESIAN_POINT('Ctrl Pts',(0.870146645090731,-0.0609922781173484,
-0.530395067942936));
#17584=CARTESIAN_POINT('Ctrl Pts',(0.871530771444223,-0.0476300000000001,
-0.528110872004958));
#17585=CARTESIAN_POINT('',(0.989696097314,-0.04763,-0.242834539687906));
#17586=CARTESIAN_POINT('Origin',(0.,-0.04763,0.));
#17587=CARTESIAN_POINT('',(0.989696097314,-0.04763,0.242834539687906));
#17588=CARTESIAN_POINT('Ctrl Pts',(0.989696097314,-0.04763,-0.242834539687907));
#17589=CARTESIAN_POINT('Ctrl Pts',(0.990332542620729,-0.0609922781173483,
-0.24024064412003));
#17590=CARTESIAN_POINT('Ctrl Pts',(0.991238884025248,-0.0742967091364493,
-0.236509675094874));
#17591=CARTESIAN_POINT('Ctrl Pts',(0.994830026707808,-0.115492077056649,
-0.221129100087819));
#17592=CARTESIAN_POINT('Ctrl Pts',(0.998375294985966,-0.141695629206859,
-0.205111543747588));
#17593=CARTESIAN_POINT('Ctrl Pts',(1.00492400591205,-0.181890537957859,
-0.169940289819232));
#17594=CARTESIAN_POINT('Ctrl Pts',(1.00869718865384,-0.201072148666545,
-0.1465689792446));
#17595=CARTESIAN_POINT('Ctrl Pts',(1.01358704779679,-0.223955109275652,
-0.106909345252087));
#17596=CARTESIAN_POINT('Ctrl Pts',(1.0156297872271,-0.232742381310829,-0.0861971848975942));
#17597=CARTESIAN_POINT('Ctrl Pts',(1.01837060663223,-0.244234834628584,
-0.0430711894098823));
#17598=CARTESIAN_POINT('Ctrl Pts',(1.019052,-0.246942143572133,-0.0206568624125607));
#17599=CARTESIAN_POINT('Ctrl Pts',(1.019052,-0.246942143572133,0.0206568624125607));
#17600=CARTESIAN_POINT('Ctrl Pts',(1.01837060663223,-0.244234834628584,
0.0430711894098823));
#17601=CARTESIAN_POINT('Ctrl Pts',(1.0156297872271,-0.232742381310829,0.0861971848975942));
#17602=CARTESIAN_POINT('Ctrl Pts',(1.01358704779679,-0.223955109275652,
0.106909345252087));
#17603=CARTESIAN_POINT('Ctrl Pts',(1.00869718865384,-0.201072148666545,
0.1465689792446));
#17604=CARTESIAN_POINT('Ctrl Pts',(1.00492400591205,-0.181890537957859,
0.169940289819232));
#17605=CARTESIAN_POINT('Ctrl Pts',(0.998375294985966,-0.141695629206859,
0.205111543747588));
#17606=CARTESIAN_POINT('Ctrl Pts',(0.994830026707808,-0.115492077056649,
0.221129100087819));
#17607=CARTESIAN_POINT('Ctrl Pts',(0.991238884025248,-0.0742967091364492,
0.236509675094874));
#17608=CARTESIAN_POINT('Ctrl Pts',(0.990332542620729,-0.0609922781173483,
0.24024064412003));
#17609=CARTESIAN_POINT('Ctrl Pts',(0.989696097314,-0.04763,0.242834539687907));
#17610=CARTESIAN_POINT('Origin',(0.,-0.04763,0.));
#17611=CARTESIAN_POINT('Origin',(0.,-0.04763,0.));
#17612=CARTESIAN_POINT('',(0.238183666596899,-0.04763,0.951592097314));
#17613=CARTESIAN_POINT('Origin',(0.,-0.04763,0.));
#17614=CARTESIAN_POINT('Origin',(-1.94289029309402E-16,-0.04763,1.));
#17615=CARTESIAN_POINT('Origin',(-1.94289029309402E-16,0.,1.));
#17616=CARTESIAN_POINT('',(-0.2381836665969,-0.04763,0.951592097314));
#17617=CARTESIAN_POINT('Ctrl Pts',(-0.238183666596899,-0.0476299999999999,
0.951592097314));
#17618=CARTESIAN_POINT('Ctrl Pts',(-0.233157223576062,-0.0740444353928835,
0.952850216871763));
#17619=CARTESIAN_POINT('Ctrl Pts',(-0.223801617934946,-0.0999305678883309,
0.955173119738174));
#17620=CARTESIAN_POINT('Ctrl Pts',(-0.199966927975188,-0.142345102874864,
0.960411259488514));
#17621=CARTESIAN_POINT('Ctrl Pts',(-0.1868781821531,-0.159766064500479,
0.963103647174702));
#17622=CARTESIAN_POINT('Ctrl Pts',(-0.15681442133453,-0.190326085855194,
0.968453058988463));
#17623=CARTESIAN_POINT('Ctrl Pts',(-0.139836317888043,-0.203463743702801,
0.971100730005489));
#17624=CARTESIAN_POINT('Ctrl Pts',(-0.104422493053067,-0.224161999508995,
0.975530745318961));
#17625=CARTESIAN_POINT('Ctrl Pts',(-0.0842175114474176,-0.232861760990032,
0.977553872336861));
#17626=CARTESIAN_POINT('Ctrl Pts',(-0.0421062857595701,-0.244251601209411,
0.980270995488453));
#17627=CARTESIAN_POINT('Ctrl Pts',(-0.0201990724523197,-0.246942143572133,
0.980948));
#17628=CARTESIAN_POINT('Ctrl Pts',(0.020199072452319,-0.246942143572133,
0.980948));
#17629=CARTESIAN_POINT('Ctrl Pts',(0.0421062857595694,-0.244251601209411,
0.980270995488454));
#17630=CARTESIAN_POINT('Ctrl Pts',(0.0842175114474169,-0.232861760990032,
0.977553872336861));
#17631=CARTESIAN_POINT('Ctrl Pts',(0.104422493053067,-0.224161999508995,
0.975530745318961));
#17632=CARTESIAN_POINT('Ctrl Pts',(0.139836317888042,-0.203463743702801,
0.971100730005489));
#17633=CARTESIAN_POINT('Ctrl Pts',(0.15681442133453,-0.190326085855194,
0.968453058988463));
#17634=CARTESIAN_POINT('Ctrl Pts',(0.1868781821531,-0.15976606450048,0.963103647174702));
#17635=CARTESIAN_POINT('Ctrl Pts',(0.199966927975188,-0.142345102874864,
0.960411259488514));
#17636=CARTESIAN_POINT('Ctrl Pts',(0.223801617934945,-0.0999305678883309,
0.955173119738174));
#17637=CARTESIAN_POINT('Ctrl Pts',(0.233157223576061,-0.0740444353928835,
0.952850216871763));
#17638=CARTESIAN_POINT('Ctrl Pts',(0.238183666596899,-0.0476299999999999,
0.951592097314));
#17639=CARTESIAN_POINT('Origin',(-1.94289029309402E-16,-0.04763,1.));
#17640=CARTESIAN_POINT('Origin',(0.,-0.04763,0.));
#17641=CARTESIAN_POINT('',(-0.504455939115715,-0.04763,0.841298510752802));
#17642=CARTESIAN_POINT('Origin',(0.,-0.04763,0.));
#17643=CARTESIAN_POINT('Origin',(-0.707106781186548,-0.04763,0.707106781186547));
#17644=CARTESIAN_POINT('Origin',(-0.707106781186548,0.,0.707106781186547));
#17645=CARTESIAN_POINT('',(-0.841298510752802,-0.04763,0.504455939115715));
#17646=CARTESIAN_POINT('Ctrl Pts',(-0.841298510752802,-0.04763,0.504455939115715));
#17647=CARTESIAN_POINT('Ctrl Pts',(-0.838633903678357,-0.0740444353928835,
0.508899795931835));
#17648=CARTESIAN_POINT('Ctrl Pts',(-0.833661031856294,-0.0999305678883309,
0.517157748491652));
#17649=CARTESIAN_POINT('Ctrl Pts',(-0.820511285096538,-0.142345102874864,
0.537715343527944));
#17650=CARTESIAN_POINT('Ctrl Pts',(-0.813159949759,-0.159766064500479,0.548874290046456));
#17651=CARTESIAN_POINT('Ctrl Pts',(-0.795684265985089,-0.190326085855194,
0.573915184558107));
#17652=CARTESIAN_POINT('Ctrl Pts',(-0.78555112003688,-0.203463743702801,
0.587792702767295));
#17653=CARTESIAN_POINT('Ctrl Pts',(-0.763642258217233,-0.224161999508995,
0.615966552324775));
#17654=CARTESIAN_POINT('Ctrl Pts',(-0.750785745543687,-0.232861760990032,
0.631684198665438));
#17655=CARTESIAN_POINT('Ctrl Pts',(-0.722929908501543,-0.244251601209411,
0.663382628119203));
#17656=CARTESIAN_POINT('Ctrl Pts',(-0.707917883896095,-0.246942143572133,
0.679352081686668));
#17657=CARTESIAN_POINT('Ctrl Pts',(-0.679352081686668,-0.246942143572133,
0.707917883896095));
#17658=CARTESIAN_POINT('Ctrl Pts',(-0.663382628119203,-0.244251601209411,
0.722929908501544));
#17659=CARTESIAN_POINT('Ctrl Pts',(-0.631684198665438,-0.232861760990031,
0.750785745543687));
#17660=CARTESIAN_POINT('Ctrl Pts',(-0.615966552324775,-0.224161999508995,
0.763642258217233));
#17661=CARTESIAN_POINT('Ctrl Pts',(-0.587792702767295,-0.203463743702801,
0.78555112003688));
#17662=CARTESIAN_POINT('Ctrl Pts',(-0.573915184558107,-0.190326085855194,
0.795684265985088));
#17663=CARTESIAN_POINT('Ctrl Pts',(-0.548874290046456,-0.159766064500479,
0.813159949759));
#17664=CARTESIAN_POINT('Ctrl Pts',(-0.537715343527944,-0.142345102874864,
0.820511285096538));
#17665=CARTESIAN_POINT('Ctrl Pts',(-0.517157748491652,-0.0999305678883309,
0.833661031856294));
#17666=CARTESIAN_POINT('Ctrl Pts',(-0.508899795931835,-0.0740444353928835,
0.838633903678357));
#17667=CARTESIAN_POINT('Ctrl Pts',(-0.504455939115716,-0.04763,0.841298510752801));
#17668=CARTESIAN_POINT('Origin',(-0.707106781186548,-0.04763,0.707106781186547));
#17669=CARTESIAN_POINT('Origin',(0.,-0.04763,0.));
#17670=CARTESIAN_POINT('',(-0.951592097314,-0.04763,0.238183666596899));
#17671=CARTESIAN_POINT('Origin',(0.,-0.04763,0.));
#17672=CARTESIAN_POINT('Origin',(-1.,-0.04763,-1.11022302462516E-16));
#17673=CARTESIAN_POINT('Origin',(-1.,0.,-1.11022302462516E-16));
#17674=CARTESIAN_POINT('',(-0.951592097314,-0.04763,-0.2381836665969));
#17675=CARTESIAN_POINT('',(-0.980948,-0.246942143572133,1.08514323328844E-18));
#17676=CARTESIAN_POINT('Ctrl Pts',(-0.951592097314,-0.04763,-0.238183666596899));
#17677=CARTESIAN_POINT('Ctrl Pts',(-0.952850216871763,-0.0740444353928835,
-0.233157223576062));
#17678=CARTESIAN_POINT('Ctrl Pts',(-0.955173119738174,-0.0999305678883309,
-0.223801617934946));
#17679=CARTESIAN_POINT('Ctrl Pts',(-0.960411259488514,-0.142345102874864,
-0.199966927975188));
#17680=CARTESIAN_POINT('Ctrl Pts',(-0.963103647174702,-0.159766064500479,
-0.1868781821531));
#17681=CARTESIAN_POINT('Ctrl Pts',(-0.968453058988463,-0.190326085855194,
-0.15681442133453));
#17682=CARTESIAN_POINT('Ctrl Pts',(-0.971100730005489,-0.203463743702801,
-0.139836317888043));
#17683=CARTESIAN_POINT('Ctrl Pts',(-0.975530745318961,-0.224161999508995,
-0.104422493053067));
#17684=CARTESIAN_POINT('Ctrl Pts',(-0.977553872336861,-0.232861760990032,
-0.0842175114474175));
#17685=CARTESIAN_POINT('Ctrl Pts',(-0.980270995488453,-0.244251601209411,
-0.0421062857595699));
#17686=CARTESIAN_POINT('Ctrl Pts',(-0.980948,-0.246942143572133,-0.0201990724523195));
#17687=CARTESIAN_POINT('Ctrl Pts',(-0.980948,-0.246942143572133,-1.17961196366423E-16));
#17688=CARTESIAN_POINT('Origin',(-1.,-0.04763,-1.11022302462516E-16));
#17689=CARTESIAN_POINT('Ctrl Pts',(-0.980948,-0.246942143572133,-1.17961196366423E-16));
#17690=CARTESIAN_POINT('Ctrl Pts',(-0.980948,-0.246942143572133,0.0201990724523192));
#17691=CARTESIAN_POINT('Ctrl Pts',(-0.980270995488453,-0.244251601209411,
0.0421062857595695));
#17692=CARTESIAN_POINT('Ctrl Pts',(-0.977553872336861,-0.232861760990032,
0.0842175114474169));
#17693=CARTESIAN_POINT('Ctrl Pts',(-0.975530745318961,-0.224161999508995,
0.104422493053066));
#17694=CARTESIAN_POINT('Ctrl Pts',(-0.971100730005489,-0.203463743702801,
0.139836317888042));
#17695=CARTESIAN_POINT('Ctrl Pts',(-0.968453058988463,-0.190326085855194,
0.15681442133453));
#17696=CARTESIAN_POINT('Ctrl Pts',(-0.963103647174702,-0.15976606450048,
0.1868781821531));
#17697=CARTESIAN_POINT('Ctrl Pts',(-0.960411259488514,-0.142345102874864,
0.199966927975188));
#17698=CARTESIAN_POINT('Ctrl Pts',(-0.955173119738174,-0.099930567888331,
0.223801617934945));
#17699=CARTESIAN_POINT('Ctrl Pts',(-0.952850216871763,-0.0740444353928835,
0.233157223576061));
#17700=CARTESIAN_POINT('Ctrl Pts',(-0.951592097314,-0.04763,0.238183666596899));
#17701=CARTESIAN_POINT('Origin',(0.,-0.04763,0.));
#17702=CARTESIAN_POINT('',(-0.841298510752802,-0.04763,-0.504455939115715));
#17703=CARTESIAN_POINT('Origin',(0.,-0.04763,0.));
#17704=CARTESIAN_POINT('Origin',(-0.707106781186547,-0.04763,-0.707106781186548));
#17705=CARTESIAN_POINT('Origin',(-0.707106781186547,0.,-0.707106781186548));
#17706=CARTESIAN_POINT('',(-0.504455939115715,-0.04763,-0.841298510752802));
#17707=CARTESIAN_POINT('Ctrl Pts',(-0.504455939115715,-0.04763,-0.841298510752802));
#17708=CARTESIAN_POINT('Ctrl Pts',(-0.508899795931835,-0.0740444353928835,
-0.838633903678357));
#17709=CARTESIAN_POINT('Ctrl Pts',(-0.517157748491652,-0.0999305678883309,
-0.833661031856294));
#17710=CARTESIAN_POINT('Ctrl Pts',(-0.537715343527944,-0.142345102874864,
-0.820511285096538));
#17711=CARTESIAN_POINT('Ctrl Pts',(-0.548874290046456,-0.159766064500479,
-0.813159949759));
#17712=CARTESIAN_POINT('Ctrl Pts',(-0.573915184558107,-0.190326085855194,
-0.795684265985089));
#17713=CARTESIAN_POINT('Ctrl Pts',(-0.587792702767295,-0.203463743702801,
-0.78555112003688));
#17714=CARTESIAN_POINT('Ctrl Pts',(-0.615966552324775,-0.224161999508995,
-0.763642258217233));
#17715=CARTESIAN_POINT('Ctrl Pts',(-0.631684198665438,-0.232861760990032,
-0.750785745543687));
#17716=CARTESIAN_POINT('Ctrl Pts',(-0.663382628119203,-0.244251601209411,
-0.722929908501543));
#17717=CARTESIAN_POINT('Ctrl Pts',(-0.679352081686668,-0.246942143572133,
-0.707917883896095));
#17718=CARTESIAN_POINT('Ctrl Pts',(-0.707917883896095,-0.246942143572133,
-0.679352081686668));
#17719=CARTESIAN_POINT('Ctrl Pts',(-0.722929908501543,-0.244251601209411,
-0.663382628119203));
#17720=CARTESIAN_POINT('Ctrl Pts',(-0.750785745543687,-0.232861760990032,
-0.631684198665439));
#17721=CARTESIAN_POINT('Ctrl Pts',(-0.763642258217232,-0.224161999508995,
-0.615966552324775));
#17722=CARTESIAN_POINT('Ctrl Pts',(-0.78555112003688,-0.203463743702801,
-0.587792702767295));
#17723=CARTESIAN_POINT('Ctrl Pts',(-0.795684265985088,-0.190326085855194,
-0.573915184558107));
#17724=CARTESIAN_POINT('Ctrl Pts',(-0.813159949759,-0.15976606450048,-0.548874290046456));
#17725=CARTESIAN_POINT('Ctrl Pts',(-0.820511285096538,-0.142345102874864,
-0.537715343527944));
#17726=CARTESIAN_POINT('Ctrl Pts',(-0.833661031856294,-0.0999305678883311,
-0.517157748491652));
#17727=CARTESIAN_POINT('Ctrl Pts',(-0.838633903678357,-0.0740444353928836,
-0.508899795931835));
#17728=CARTESIAN_POINT('Ctrl Pts',(-0.841298510752801,-0.04763,-0.504455939115715));
#17729=CARTESIAN_POINT('Origin',(-0.707106781186547,-0.04763,-0.707106781186548));
#17730=CARTESIAN_POINT('Origin',(0.,-0.04763,0.));
#17731=CARTESIAN_POINT('',(-0.238183666596899,-0.04763,-0.951592097314));
#17732=CARTESIAN_POINT('Origin',(0.,-0.04763,0.));
#17733=CARTESIAN_POINT('Origin',(5.55111512312578E-17,-0.04763,-1.));
#17734=CARTESIAN_POINT('Origin',(5.55111512312578E-17,0.,-1.));
#17735=CARTESIAN_POINT('',(0.238183666596899,-0.04763,-0.951592097314));
#17736=CARTESIAN_POINT('Ctrl Pts',(0.238183666596899,-0.04763,-0.951592097314));
#17737=CARTESIAN_POINT('Ctrl Pts',(0.233157223576062,-0.0740444353928835,
-0.952850216871763));
#17738=CARTESIAN_POINT('Ctrl Pts',(0.223801617934946,-0.099930567888331,
-0.955173119738174));
#17739=CARTESIAN_POINT('Ctrl Pts',(0.199966927975188,-0.142345102874864,
-0.960411259488514));
#17740=CARTESIAN_POINT('Ctrl Pts',(0.1868781821531,-0.15976606450048,-0.963103647174702));
#17741=CARTESIAN_POINT('Ctrl Pts',(0.15681442133453,-0.190326085855194,
-0.968453058988463));
#17742=CARTESIAN_POINT('Ctrl Pts',(0.139836317888042,-0.203463743702801,
-0.971100730005489));
#17743=CARTESIAN_POINT('Ctrl Pts',(0.104422493053067,-0.224161999508995,
-0.975530745318961));
#17744=CARTESIAN_POINT('Ctrl Pts',(0.0842175114474173,-0.232861760990032,
-0.977553872336861));
#17745=CARTESIAN_POINT('Ctrl Pts',(0.0421062857595698,-0.244251601209411,
-0.980270995488453));
#17746=CARTESIAN_POINT('Ctrl Pts',(0.0201990724523194,-0.246942143572133,
-0.980948));
#17747=CARTESIAN_POINT('Ctrl Pts',(-0.0201990724523193,-0.246942143572133,
-0.980948));
#17748=CARTESIAN_POINT('Ctrl Pts',(-0.0421062857595697,-0.244251601209411,
-0.980270995488453));
#17749=CARTESIAN_POINT('Ctrl Pts',(-0.0842175114474171,-0.232861760990032,
-0.977553872336861));
#17750=CARTESIAN_POINT('Ctrl Pts',(-0.104422493053067,-0.224161999508995,
-0.975530745318961));
#17751=CARTESIAN_POINT('Ctrl Pts',(-0.139836317888042,-0.203463743702801,
-0.971100730005489));
#17752=CARTESIAN_POINT('Ctrl Pts',(-0.15681442133453,-0.190326085855194,
-0.968453058988463));
#17753=CARTESIAN_POINT('Ctrl Pts',(-0.1868781821531,-0.15976606450048,-0.963103647174702));
#17754=CARTESIAN_POINT('Ctrl Pts',(-0.199966927975188,-0.142345102874864,
-0.960411259488514));
#17755=CARTESIAN_POINT('Ctrl Pts',(-0.223801617934945,-0.099930567888331,
-0.955173119738174));
#17756=CARTESIAN_POINT('Ctrl Pts',(-0.233157223576062,-0.0740444353928835,
-0.952850216871763));
#17757=CARTESIAN_POINT('Ctrl Pts',(-0.238183666596899,-0.0476299999999999,
-0.951592097314));
#17758=CARTESIAN_POINT('Origin',(5.55111512312578E-17,-0.04763,-1.));
#17759=CARTESIAN_POINT('Origin',(0.,-0.04763,0.));
#17760=CARTESIAN_POINT('',(0.504455939115715,-0.04763,-0.841298510752802));
#17761=CARTESIAN_POINT('Origin',(0.,-0.04763,0.));
#17762=CARTESIAN_POINT('Origin',(0.707106781186548,-0.04763,-0.707106781186547));
#17763=CARTESIAN_POINT('Origin',(0.707106781186548,0.,-0.707106781186547));
#17764=CARTESIAN_POINT('',(0.841298510752802,-0.04763,-0.504455939115715));
#17765=CARTESIAN_POINT('Ctrl Pts',(0.841298510752802,-0.04763,-0.504455939115715));
#17766=CARTESIAN_POINT('Ctrl Pts',(0.838633903678357,-0.0740444353928835,
-0.508899795931835));
#17767=CARTESIAN_POINT('Ctrl Pts',(0.833661031856294,-0.0999305678883309,
-0.517157748491652));
#17768=CARTESIAN_POINT('Ctrl Pts',(0.820511285096538,-0.142345102874864,
-0.537715343527944));
#17769=CARTESIAN_POINT('Ctrl Pts',(0.813159949759,-0.159766064500479,-0.548874290046456));
#17770=CARTESIAN_POINT('Ctrl Pts',(0.795684265985088,-0.190326085855194,
-0.573915184558107));
#17771=CARTESIAN_POINT('Ctrl Pts',(0.78555112003688,-0.203463743702801,
-0.587792702767295));
#17772=CARTESIAN_POINT('Ctrl Pts',(0.763642258217233,-0.224161999508995,
-0.615966552324775));
#17773=CARTESIAN_POINT('Ctrl Pts',(0.750785745543687,-0.232861760990032,
-0.631684198665438));
#17774=CARTESIAN_POINT('Ctrl Pts',(0.722929908501543,-0.244251601209411,
-0.663382628119203));
#17775=CARTESIAN_POINT('Ctrl Pts',(0.707917883896095,-0.246942143572133,
-0.679352081686668));
#17776=CARTESIAN_POINT('Ctrl Pts',(0.679352081686668,-0.246942143572133,
-0.707917883896095));
#17777=CARTESIAN_POINT('Ctrl Pts',(0.663382628119203,-0.244251601209411,
-0.722929908501543));
#17778=CARTESIAN_POINT('Ctrl Pts',(0.631684198665438,-0.232861760990032,
-0.750785745543687));
#17779=CARTESIAN_POINT('Ctrl Pts',(0.615966552324775,-0.224161999508995,
-0.763642258217232));
#17780=CARTESIAN_POINT('Ctrl Pts',(0.587792702767295,-0.203463743702801,
-0.78555112003688));
#17781=CARTESIAN_POINT('Ctrl Pts',(0.573915184558107,-0.190326085855194,
-0.795684265985088));
#17782=CARTESIAN_POINT('Ctrl Pts',(0.548874290046456,-0.159766064500479,
-0.813159949759));
#17783=CARTESIAN_POINT('Ctrl Pts',(0.537715343527944,-0.142345102874864,
-0.820511285096538));
#17784=CARTESIAN_POINT('Ctrl Pts',(0.517157748491652,-0.099930567888331,
-0.833661031856294));
#17785=CARTESIAN_POINT('Ctrl Pts',(0.508899795931835,-0.0740444353928835,
-0.838633903678357));
#17786=CARTESIAN_POINT('Ctrl Pts',(0.504455939115715,-0.04763,-0.841298510752801));
#17787=CARTESIAN_POINT('Origin',(0.707106781186548,-0.04763,-0.707106781186547));
#17788=CARTESIAN_POINT('Origin',(0.,-0.166705,0.));
#17789=CARTESIAN_POINT('',(-0.980948,-0.28578,1.20131482833E-16));
#17790=CARTESIAN_POINT('Origin',(0.,-0.28578,0.));
#17791=CARTESIAN_POINT('',(-0.980948,-0.166705,1.20131482833E-16));
#17792=CARTESIAN_POINT('',(0.951592097314,-0.04763,0.238183666596899));
#17793=CARTESIAN_POINT('Origin',(0.,-0.04763,0.));
#17794=CARTESIAN_POINT('',(0.951592097314,-0.04763,-0.238183666596899));
#17795=CARTESIAN_POINT('Ctrl Pts',(0.951592097314,-0.04763,0.238183666596899));
#17796=CARTESIAN_POINT('Ctrl Pts',(0.952850216871763,-0.0740444353928835,
0.233157223576062));
#17797=CARTESIAN_POINT('Ctrl Pts',(0.955173119738174,-0.099930567888331,
0.223801617934945));
#17798=CARTESIAN_POINT('Ctrl Pts',(0.960411259488514,-0.142345102874864,
0.199966927975188));
#17799=CARTESIAN_POINT('Ctrl Pts',(0.963103647174702,-0.15976606450048,
0.1868781821531));
#17800=CARTESIAN_POINT('Ctrl Pts',(0.968453058988463,-0.190326085855194,
0.15681442133453));
#17801=CARTESIAN_POINT('Ctrl Pts',(0.971100730005489,-0.203463743702801,
0.139836317888042));
#17802=CARTESIAN_POINT('Ctrl Pts',(0.975530745318961,-0.224161999508995,
0.104422493053067));
#17803=CARTESIAN_POINT('Ctrl Pts',(0.977553872336861,-0.232861760990032,
0.0842175114474172));
#17804=CARTESIAN_POINT('Ctrl Pts',(0.980270995488453,-0.244251601209411,
0.0421062857595697));
#17805=CARTESIAN_POINT('Ctrl Pts',(0.980948,-0.246942143572133,0.0201990724523194));
#17806=CARTESIAN_POINT('Ctrl Pts',(0.980948,-0.246942143572133,-0.0201990724523194));
#17807=CARTESIAN_POINT('Ctrl Pts',(0.980270995488453,-0.244251601209411,
-0.0421062857595697));
#17808=CARTESIAN_POINT('Ctrl Pts',(0.977553872336861,-0.232861760990032,
-0.0842175114474172));
#17809=CARTESIAN_POINT('Ctrl Pts',(0.975530745318961,-0.224161999508995,
-0.104422493053067));
#17810=CARTESIAN_POINT('Ctrl Pts',(0.971100730005489,-0.203463743702801,
-0.139836317888042));
#17811=CARTESIAN_POINT('Ctrl Pts',(0.968453058988463,-0.190326085855194,
-0.15681442133453));
#17812=CARTESIAN_POINT('Ctrl Pts',(0.963103647174702,-0.15976606450048,
-0.1868781821531));
#17813=CARTESIAN_POINT('Ctrl Pts',(0.960411259488514,-0.142345102874864,
-0.199966927975188));
#17814=CARTESIAN_POINT('Ctrl Pts',(0.955173119738174,-0.099930567888331,
-0.223801617934945));
#17815=CARTESIAN_POINT('Ctrl Pts',(0.952850216871763,-0.0740444353928835,
-0.233157223576062));
#17816=CARTESIAN_POINT('Ctrl Pts',(0.951592097314,-0.0476299999999999,-0.238183666596899));
#17817=CARTESIAN_POINT('Origin',(0.,-0.04763,0.));
#17818=CARTESIAN_POINT('Origin',(0.,-0.04763,0.));
#17819=CARTESIAN_POINT('Origin',(1.,-0.04763,0.));
#17820=CARTESIAN_POINT('Origin',(1.,0.,0.));
#17821=CARTESIAN_POINT('Origin',(1.,-0.04763,0.));
#17822=CARTESIAN_POINT('Origin',(0.,-0.28578,0.));
#17823=CARTESIAN_POINT('Origin',(0.,-0.04763,0.));
#17824=CARTESIAN_POINT('',(0.,0.,0.));
#17825=CARTESIAN_POINT('Origin',(1.013815,0.445,0.));
#17826=CARTESIAN_POINT('',(-1.013815,0.445,-1.24156529467757E-16));
#17827=CARTESIAN_POINT('Origin',(0.,0.445,0.));
#17828=CARTESIAN_POINT('',(-0.991185,0.445,-1.21385153761287E-16));
#17829=CARTESIAN_POINT('Origin',(0.,0.445,0.));
#17830=CARTESIAN_POINT('Origin',(0.,0.4075,0.));
#17831=CARTESIAN_POINT('',(-1.013815,0.37,-1.24156529467757E-16));
#17832=CARTESIAN_POINT('Origin',(0.,0.37,0.));
#17833=CARTESIAN_POINT('',(-1.013815,0.4075,-1.24156529467757E-16));
#17834=CARTESIAN_POINT('Origin',(0.991185,0.37,0.));
#17835=CARTESIAN_POINT('',(-0.991185,0.37,-1.21385153761287E-16));
#17836=CARTESIAN_POINT('Origin',(0.,0.37,0.));
#17837=CARTESIAN_POINT('Origin',(0.,0.4075,0.));
#17838=CARTESIAN_POINT('',(-0.991185,0.4075,-1.21385153761287E-16));
#17839=CARTESIAN_POINT('Origin',(1.013815,-0.37,0.));
#17840=CARTESIAN_POINT('',(-1.013815,-0.37,-1.24156529467757E-16));
#17841=CARTESIAN_POINT('Origin',(0.,-0.37,0.));
#17842=CARTESIAN_POINT('',(-0.991185,-0.37,-1.21385153761287E-16));
#17843=CARTESIAN_POINT('Origin',(0.,-0.37,0.));
#17844=CARTESIAN_POINT('Origin',(0.,-0.4075,0.));
#17845=CARTESIAN_POINT('',(-1.013815,-0.445,-1.24156529467757E-16));
#17846=CARTESIAN_POINT('Origin',(0.,-0.445,0.));
#17847=CARTESIAN_POINT('',(-1.013815,-0.4075,-1.24156529467757E-16));
#17848=CARTESIAN_POINT('Origin',(0.991185,-0.445,0.));
#17849=CARTESIAN_POINT('',(-0.991185,-0.445,-1.21385153761287E-16));
#17850=CARTESIAN_POINT('Origin',(0.,-0.445,0.));
#17851=CARTESIAN_POINT('Origin',(0.,-0.4075,0.));
#17852=CARTESIAN_POINT('',(-0.991185,-0.4075,-1.21385153761287E-16));
#17853=CARTESIAN_POINT('',(0.,0.,0.));
#17854=CARTESIAN_POINT('',(0.,0.,0.));
#17855=CARTESIAN_POINT('',(0.,0.,0.));
#17856=CARTESIAN_POINT('',(0.,0.,0.));
#17857=CARTESIAN_POINT('',(0.,0.,0.));
#17858=CARTESIAN_POINT('',(0.,0.,0.));
#17859=CARTESIAN_POINT('Origin',(-0.1,0.82,-0.3));
#17860=CARTESIAN_POINT('',(0.,0.82,-0.3));
#17861=CARTESIAN_POINT('',(0.,1.,-0.3));
#17862=CARTESIAN_POINT('',(0.,0.41,-0.3));
#17863=CARTESIAN_POINT('',(40.,0.82,-0.3));
#17864=CARTESIAN_POINT('',(-0.1,0.82,-0.3));
#17865=CARTESIAN_POINT('',(40.,1.,-0.3));
#17866=CARTESIAN_POINT('',(40.,0.41,-0.3));
#17867=CARTESIAN_POINT('',(-0.05,1.,-0.3));
#17868=CARTESIAN_POINT('Origin',(-0.1,0.82,-0.55));
#17869=CARTESIAN_POINT('',(0.,0.82,-0.55));
#17870=CARTESIAN_POINT('',(0.,0.82,-0.275));
#17871=CARTESIAN_POINT('',(40.,0.82,-0.55));
#17872=CARTESIAN_POINT('',(-0.1,0.82,-0.55));
#17873=CARTESIAN_POINT('',(40.,0.82,-0.275));
#17874=CARTESIAN_POINT('Origin',(-0.1,0.67,-0.55));
#17875=CARTESIAN_POINT('',(0.,0.67,-0.55));
#17876=CARTESIAN_POINT('',(0.,0.335,-0.55));
#17877=CARTESIAN_POINT('',(40.,0.67,-0.55));
#17878=CARTESIAN_POINT('',(-0.1,0.67,-0.55));
#17879=CARTESIAN_POINT('',(40.,0.335,-0.55));
#17880=CARTESIAN_POINT('Origin',(-0.1,0.42,-0.3));
#17881=CARTESIAN_POINT('',(0.,0.42,-0.3));
#17882=CARTESIAN_POINT('',(0.,0.24,-0.12));
#17883=CARTESIAN_POINT('',(40.,0.42,-0.3));
#17884=CARTESIAN_POINT('',(-0.1,0.42,-0.3));
#17885=CARTESIAN_POINT('',(40.,0.24,-0.12));
#17886=CARTESIAN_POINT('Origin',(-0.1,0.42,0.3));
#17887=CARTESIAN_POINT('',(0.,0.42,0.3));
#17888=CARTESIAN_POINT('',(0.,0.42,0.15));
#17889=CARTESIAN_POINT('',(40.,0.42,0.3));
#17890=CARTESIAN_POINT('',(-0.1,0.42,0.3));
#17891=CARTESIAN_POINT('',(40.,0.42,0.15));
#17892=CARTESIAN_POINT('Origin',(-0.1,0.67,0.55));
#17893=CARTESIAN_POINT('',(0.,0.67,0.55));
#17894=CARTESIAN_POINT('',(6.93889390390723E-18,0.365,0.245));
#17895=CARTESIAN_POINT('',(40.,0.67,0.55));
#17896=CARTESIAN_POINT('',(-0.1,0.67,0.55));
#17897=CARTESIAN_POINT('',(40.,0.365,0.245));
#17898=CARTESIAN_POINT('Origin',(-0.1,0.82,0.55));
#17899=CARTESIAN_POINT('',(0.,0.82,0.55));
#17900=CARTESIAN_POINT('',(0.,0.41,0.55));
#17901=CARTESIAN_POINT('',(40.,0.82,0.55));
#17902=CARTESIAN_POINT('',(-0.1,0.82,0.55));
#17903=CARTESIAN_POINT('',(40.,0.41,0.55));
#17904=CARTESIAN_POINT('Origin',(-0.1,0.82,0.3));
#17905=CARTESIAN_POINT('',(0.,0.82,0.3));
#17906=CARTESIAN_POINT('',(0.,0.82,0.15));
#17907=CARTESIAN_POINT('',(40.,0.82,0.3));
#17908=CARTESIAN_POINT('',(-0.1,0.82,0.3));
#17909=CARTESIAN_POINT('',(40.,0.82,0.15));
#17910=CARTESIAN_POINT('Origin',(-0.1,1.05,0.3));
#17911=CARTESIAN_POINT('',(0.,1.,0.3));
#17912=CARTESIAN_POINT('',(0.,0.525,0.3));
#17913=CARTESIAN_POINT('',(40.,1.,0.3));
#17914=CARTESIAN_POINT('',(-0.05,1.,0.3));
#17915=CARTESIAN_POINT('',(40.,0.525,0.3));
#17916=CARTESIAN_POINT('Origin',(-0.1,-0.3,-0.82));
#17917=CARTESIAN_POINT('',(0.,-0.3,-0.82));
#17918=CARTESIAN_POINT('',(0.,-0.3,-1.));
#17919=CARTESIAN_POINT('',(0.,-0.3,-0.41));
#17920=CARTESIAN_POINT('',(40.,-0.3,-0.82));
#17921=CARTESIAN_POINT('',(-0.1,-0.3,-0.82));
#17922=CARTESIAN_POINT('',(40.,-0.3,-1.));
#17923=CARTESIAN_POINT('',(40.,-0.3,-0.41));
#17924=CARTESIAN_POINT('',(-0.05,-0.3,-1.));
#17925=CARTESIAN_POINT('Origin',(-0.1,-0.55,-0.82));
#17926=CARTESIAN_POINT('',(0.,-0.55,-0.82));
#17927=CARTESIAN_POINT('',(0.,-0.275,-0.82));
#17928=CARTESIAN_POINT('',(40.,-0.55,-0.82));
#17929=CARTESIAN_POINT('',(-0.1,-0.55,-0.82));
#17930=CARTESIAN_POINT('',(40.,-0.275,-0.82));
#17931=CARTESIAN_POINT('Origin',(-0.1,-0.55,-0.67));
#17932=CARTESIAN_POINT('',(0.,-0.55,-0.67));
#17933=CARTESIAN_POINT('',(0.,-0.55,-0.335));
#17934=CARTESIAN_POINT('',(40.,-0.55,-0.67));
#17935=CARTESIAN_POINT('',(-0.1,-0.55,-0.67));
#17936=CARTESIAN_POINT('',(40.,-0.55,-0.335));
#17937=CARTESIAN_POINT('Origin',(-0.1,-0.3,-0.42));
#17938=CARTESIAN_POINT('',(0.,-0.3,-0.42));
#17939=CARTESIAN_POINT('',(0.,-0.12,-0.24));
#17940=CARTESIAN_POINT('',(40.,-0.3,-0.42));
#17941=CARTESIAN_POINT('',(-0.1,-0.3,-0.42));
#17942=CARTESIAN_POINT('',(40.,-0.12,-0.24));
#17943=CARTESIAN_POINT('Origin',(-0.1,0.3,-0.42));
#17944=CARTESIAN_POINT('',(0.,0.3,-0.42));
#17945=CARTESIAN_POINT('',(0.,0.15,-0.42));
#17946=CARTESIAN_POINT('',(40.,0.3,-0.42));
#17947=CARTESIAN_POINT('',(-0.1,0.3,-0.42));
#17948=CARTESIAN_POINT('',(40.,0.15,-0.42));
#17949=CARTESIAN_POINT('Origin',(-0.1,0.55,-0.67));
#17950=CARTESIAN_POINT('',(0.,0.55,-0.67));
#17951=CARTESIAN_POINT('',(0.,0.245,-0.365));
#17952=CARTESIAN_POINT('',(40.,0.55,-0.67));
#17953=CARTESIAN_POINT('',(-0.1,0.55,-0.67));
#17954=CARTESIAN_POINT('',(40.,0.245,-0.365));
#17955=CARTESIAN_POINT('Origin',(-0.1,0.55,-0.82));
#17956=CARTESIAN_POINT('',(0.,0.55,-0.82));
#17957=CARTESIAN_POINT('',(0.,0.55,-0.41));
#17958=CARTESIAN_POINT('',(40.,0.55,-0.82));
#17959=CARTESIAN_POINT('',(-0.1,0.55,-0.82));
#17960=CARTESIAN_POINT('',(40.,0.55,-0.41));
#17961=CARTESIAN_POINT('Origin',(-0.1,0.3,-0.82));
#17962=CARTESIAN_POINT('',(0.,0.3,-0.82));
#17963=CARTESIAN_POINT('',(0.,0.15,-0.82));
#17964=CARTESIAN_POINT('',(40.,0.3,-0.82));
#17965=CARTESIAN_POINT('',(-0.1,0.3,-0.82));
#17966=CARTESIAN_POINT('',(40.,0.15,-0.82));
#17967=CARTESIAN_POINT('Origin',(-0.1,0.3,-1.05));
#17968=CARTESIAN_POINT('',(0.,0.3,-1.));
#17969=CARTESIAN_POINT('',(0.,0.3,-0.525));
#17970=CARTESIAN_POINT('',(40.,0.3,-1.));
#17971=CARTESIAN_POINT('',(-0.05,0.3,-1.));
#17972=CARTESIAN_POINT('',(40.,0.3,-0.525));
#17973=CARTESIAN_POINT('Origin',(-0.1,-0.82,0.3));
#17974=CARTESIAN_POINT('',(0.,-0.82,0.3));
#17975=CARTESIAN_POINT('',(0.,-1.,0.3));
#17976=CARTESIAN_POINT('',(0.,-0.41,0.3));
#17977=CARTESIAN_POINT('',(40.,-0.82,0.3));
#17978=CARTESIAN_POINT('',(-0.1,-0.82,0.3));
#17979=CARTESIAN_POINT('',(40.,-1.,0.3));
#17980=CARTESIAN_POINT('',(40.,-0.41,0.3));
#17981=CARTESIAN_POINT('',(-0.05,-1.,0.3));
#17982=CARTESIAN_POINT('Origin',(-0.1,-0.82,0.55));
#17983=CARTESIAN_POINT('',(0.,-0.82,0.55));
#17984=CARTESIAN_POINT('',(0.,-0.82,0.275));
#17985=CARTESIAN_POINT('',(40.,-0.82,0.55));
#17986=CARTESIAN_POINT('',(-0.1,-0.82,0.55));
#17987=CARTESIAN_POINT('',(40.,-0.82,0.275));
#17988=CARTESIAN_POINT('Origin',(-0.1,-0.67,0.55));
#17989=CARTESIAN_POINT('',(0.,-0.67,0.55));
#17990=CARTESIAN_POINT('',(0.,-0.335,0.55));
#17991=CARTESIAN_POINT('',(40.,-0.67,0.55));
#17992=CARTESIAN_POINT('',(-0.1,-0.67,0.55));
#17993=CARTESIAN_POINT('',(40.,-0.335,0.55));
#17994=CARTESIAN_POINT('Origin',(-0.1,-0.42,0.3));
#17995=CARTESIAN_POINT('',(0.,-0.42,0.3));
#17996=CARTESIAN_POINT('',(-6.93889390390723E-18,-0.24,0.12));
#17997=CARTESIAN_POINT('',(40.,-0.42,0.3));
#17998=CARTESIAN_POINT('',(-0.1,-0.42,0.3));
#17999=CARTESIAN_POINT('',(40.,-0.24,0.12));
#18000=CARTESIAN_POINT('Origin',(-0.1,-0.42,-0.3));
#18001=CARTESIAN_POINT('',(0.,-0.42,-0.3));
#18002=CARTESIAN_POINT('',(0.,-0.42,-0.15));
#18003=CARTESIAN_POINT('',(40.,-0.42,-0.3));
#18004=CARTESIAN_POINT('',(-0.1,-0.42,-0.3));
#18005=CARTESIAN_POINT('',(40.,-0.42,-0.15));
#18006=CARTESIAN_POINT('Origin',(-0.1,-0.67,-0.55));
#18007=CARTESIAN_POINT('',(0.,-0.67,-0.55));
#18008=CARTESIAN_POINT('',(0.,-0.365,-0.245));
#18009=CARTESIAN_POINT('',(40.,-0.67,-0.55));
#18010=CARTESIAN_POINT('',(-0.1,-0.67,-0.55));
#18011=CARTESIAN_POINT('',(40.,-0.365,-0.245));
#18012=CARTESIAN_POINT('Origin',(-0.1,-0.82,-0.55));
#18013=CARTESIAN_POINT('',(0.,-0.82,-0.55));
#18014=CARTESIAN_POINT('',(0.,-0.41,-0.55));
#18015=CARTESIAN_POINT('',(40.,-0.82,-0.55));
#18016=CARTESIAN_POINT('',(-0.1,-0.82,-0.55));
#18017=CARTESIAN_POINT('',(40.,-0.41,-0.55));
#18018=CARTESIAN_POINT('Origin',(-0.1,-0.82,-0.3));
#18019=CARTESIAN_POINT('',(0.,-0.82,-0.3));
#18020=CARTESIAN_POINT('',(0.,-0.82,-0.15));
#18021=CARTESIAN_POINT('',(40.,-0.82,-0.3));
#18022=CARTESIAN_POINT('',(-0.1,-0.82,-0.3));
#18023=CARTESIAN_POINT('',(40.,-0.82,-0.15));
#18024=CARTESIAN_POINT('Origin',(-0.1,-1.05,-0.3));
#18025=CARTESIAN_POINT('',(0.,-1.,-0.3));
#18026=CARTESIAN_POINT('',(0.,-0.525,-0.3));
#18027=CARTESIAN_POINT('',(40.,-1.,-0.3));
#18028=CARTESIAN_POINT('',(-0.05,-1.,-0.3));
#18029=CARTESIAN_POINT('',(40.,-0.525,-0.3));
#18030=CARTESIAN_POINT('Origin',(-0.1,0.3,0.82));
#18031=CARTESIAN_POINT('',(0.,0.3,0.82));
#18032=CARTESIAN_POINT('',(0.,0.3,1.));
#18033=CARTESIAN_POINT('',(0.,0.3,0.41));
#18034=CARTESIAN_POINT('',(40.,0.3,0.82));
#18035=CARTESIAN_POINT('',(-0.1,0.3,0.82));
#18036=CARTESIAN_POINT('',(40.,0.3,1.));
#18037=CARTESIAN_POINT('',(40.,0.3,0.41));
#18038=CARTESIAN_POINT('',(-0.05,0.3,1.));
#18039=CARTESIAN_POINT('Origin',(-0.1,0.55,0.82));
#18040=CARTESIAN_POINT('',(0.,0.55,0.82));
#18041=CARTESIAN_POINT('',(0.,0.275,0.82));
#18042=CARTESIAN_POINT('',(40.,0.55,0.82));
#18043=CARTESIAN_POINT('',(-0.1,0.55,0.82));
#18044=CARTESIAN_POINT('',(40.,0.275,0.82));
#18045=CARTESIAN_POINT('Origin',(-0.1,0.55,0.67));
#18046=CARTESIAN_POINT('',(0.,0.55,0.67));
#18047=CARTESIAN_POINT('',(0.,0.55,0.335));
#18048=CARTESIAN_POINT('',(40.,0.55,0.67));
#18049=CARTESIAN_POINT('',(-0.1,0.55,0.67));
#18050=CARTESIAN_POINT('',(40.,0.55,0.335));
#18051=CARTESIAN_POINT('Origin',(-0.1,0.3,0.42));
#18052=CARTESIAN_POINT('',(0.,0.3,0.42));
#18053=CARTESIAN_POINT('',(6.93889390390723E-18,0.12,0.24));
#18054=CARTESIAN_POINT('',(40.,0.3,0.42));
#18055=CARTESIAN_POINT('',(-0.1,0.3,0.42));
#18056=CARTESIAN_POINT('',(40.,0.12,0.24));
#18057=CARTESIAN_POINT('Origin',(-0.1,-0.3,0.42));
#18058=CARTESIAN_POINT('',(0.,-0.3,0.42));
#18059=CARTESIAN_POINT('',(0.,-0.15,0.42));
#18060=CARTESIAN_POINT('',(40.,-0.3,0.42));
#18061=CARTESIAN_POINT('',(-0.1,-0.3,0.42));
#18062=CARTESIAN_POINT('',(40.,-0.15,0.42));
#18063=CARTESIAN_POINT('Origin',(-0.1,-0.55,0.67));
#18064=CARTESIAN_POINT('',(0.,-0.55,0.67));
#18065=CARTESIAN_POINT('',(6.93889390390723E-18,-0.245,0.365));
#18066=CARTESIAN_POINT('',(40.,-0.55,0.67));
#18067=CARTESIAN_POINT('',(-0.1,-0.55,0.67));
#18068=CARTESIAN_POINT('',(40.,-0.245,0.365));
#18069=CARTESIAN_POINT('Origin',(-0.1,-0.55,0.82));
#18070=CARTESIAN_POINT('',(0.,-0.55,0.82));
#18071=CARTESIAN_POINT('',(0.,-0.55,0.41));
#18072=CARTESIAN_POINT('',(40.,-0.55,0.82));
#18073=CARTESIAN_POINT('',(-0.1,-0.55,0.82));
#18074=CARTESIAN_POINT('',(40.,-0.55,0.41));
#18075=CARTESIAN_POINT('Origin',(-0.1,-0.3,0.82));
#18076=CARTESIAN_POINT('',(0.,-0.3,0.82));
#18077=CARTESIAN_POINT('',(0.,-0.15,0.82));
#18078=CARTESIAN_POINT('',(40.,-0.3,0.82));
#18079=CARTESIAN_POINT('',(-0.1,-0.3,0.82));
#18080=CARTESIAN_POINT('',(40.,-0.15,0.82));
#18081=CARTESIAN_POINT('Origin',(-0.1,-0.3,1.05));
#18082=CARTESIAN_POINT('',(0.,-0.3,1.));
#18083=CARTESIAN_POINT('',(0.,-0.3,0.525));
#18084=CARTESIAN_POINT('',(40.,-0.3,1.));
#18085=CARTESIAN_POINT('',(-0.05,-0.3,1.));
#18086=CARTESIAN_POINT('',(40.,-0.3,0.525));
#18087=CARTESIAN_POINT('Origin',(-0.1,0.,0.));
#18088=CARTESIAN_POINT('',(0.,-2.57175827820944E-17,0.21));
#18089=CARTESIAN_POINT('Origin',(0.,0.,0.));
#18090=CARTESIAN_POINT('',(40.,2.57175827820944E-17,0.21));
#18091=CARTESIAN_POINT('',(-0.1,-2.57175827820944E-17,0.21));
#18092=CARTESIAN_POINT('Origin',(40.,0.,0.));
#18093=CARTESIAN_POINT('Origin',(0.,1.,-1.));
#18094=CARTESIAN_POINT('',(0.,1.,1.));
#18095=CARTESIAN_POINT('',(0.,1.,-1.));
#18096=CARTESIAN_POINT('',(40.,1.,1.));
#18097=CARTESIAN_POINT('',(0.,1.,1.));
#18098=CARTESIAN_POINT('',(40.,1.,-1.));
#18099=CARTESIAN_POINT('Origin',(0.,1.,-1.));
#18100=CARTESIAN_POINT('',(40.,1.,-1.));
#18101=CARTESIAN_POINT('',(40.,1.,-1.));
#18102=CARTESIAN_POINT('',(0.,1.,-1.));
#18103=CARTESIAN_POINT('',(0.,1.,-1.));
#18104=CARTESIAN_POINT('',(0.,1.,-1.));
#18105=CARTESIAN_POINT('Origin',(0.,-1.,-1.));
#18106=CARTESIAN_POINT('',(0.,-1.,-1.));
#18107=CARTESIAN_POINT('',(40.,-1.,-1.));
#18108=CARTESIAN_POINT('Origin',(0.,-1.,-1.));
#18109=CARTESIAN_POINT('',(40.,-1.,-1.));
#18110=CARTESIAN_POINT('',(40.,-1.,-1.));
#18111=CARTESIAN_POINT('',(0.,-1.,-1.));
#18112=CARTESIAN_POINT('',(0.,-1.,-1.));
#18113=CARTESIAN_POINT('',(0.,-1.,-1.));
#18114=CARTESIAN_POINT('Origin',(0.,-1.,1.));
#18115=CARTESIAN_POINT('',(0.,-1.,1.));
#18116=CARTESIAN_POINT('',(40.,-1.,1.));
#18117=CARTESIAN_POINT('Origin',(0.,-1.,1.));
#18118=CARTESIAN_POINT('',(40.,-1.,1.));
#18119=CARTESIAN_POINT('',(40.,-1.,1.));
#18120=CARTESIAN_POINT('',(0.,-1.,1.));
#18121=CARTESIAN_POINT('',(0.,-1.,1.));
#18122=CARTESIAN_POINT('',(0.,-1.,1.));
#18123=CARTESIAN_POINT('Origin',(0.,1.,1.));
#18124=CARTESIAN_POINT('',(0.,1.,1.));
#18125=CARTESIAN_POINT('',(40.,1.,1.));
#18126=CARTESIAN_POINT('Origin',(0.,1.,1.));
#18127=CARTESIAN_POINT('',(40.,1.,1.));
#18128=CARTESIAN_POINT('',(0.,1.,1.));
#18129=CARTESIAN_POINT('Origin',(40.,0.,0.));
#18130=CARTESIAN_POINT('Origin',(0.,0.,0.));
#18131=CARTESIAN_POINT('',(0.,0.,0.));
#18132=CARTESIAN_POINT('Origin',(0.,0.395,0.25));
#18133=CARTESIAN_POINT('',(-0.5,0.3,0.25));
#18134=CARTESIAN_POINT('',(0.5,0.3,0.25));
#18135=CARTESIAN_POINT('',(0.25,0.3,0.25));
#18136=CARTESIAN_POINT('',(-0.5,0.5,0.25));
#18137=CARTESIAN_POINT('',(-0.5,0.5,0.25));
#18138=CARTESIAN_POINT('',(0.5,0.5,0.25));
#18139=CARTESIAN_POINT('',(0.5,0.5,0.25));
#18140=CARTESIAN_POINT('',(0.5,0.29,0.25));
#18141=CARTESIAN_POINT('Origin',(0.5,0.5,0.25));
#18142=CARTESIAN_POINT('',(-0.5,0.5,0.4));
#18143=CARTESIAN_POINT('',(-0.5,0.5,0.25));
#18144=CARTESIAN_POINT('',(0.5,0.5,0.4));
#18145=CARTESIAN_POINT('',(0.5,0.5,0.4));
#18146=CARTESIAN_POINT('',(0.5,0.5,0.25));
#18147=CARTESIAN_POINT('Origin',(0.,0.,0.4));
#18148=CARTESIAN_POINT('',(-0.5,-0.5,0.4));
#18149=CARTESIAN_POINT('',(-0.5,0.5,0.4));
#18150=CARTESIAN_POINT('',(0.5,-0.5,0.4));
#18151=CARTESIAN_POINT('',(-0.5,-0.5,0.4));
#18152=CARTESIAN_POINT('',(0.5,-0.3,0.4));
#18153=CARTESIAN_POINT('',(-0.2117,2.59257727379495E-17,0.4));
#18154=CARTESIAN_POINT('Origin',(0.,0.,0.4));
#18155=CARTESIAN_POINT('Origin',(-0.5,0.3,0.));
#18156=CARTESIAN_POINT('',(-0.5,0.3,0.15));
#18157=CARTESIAN_POINT('',(-0.5,0.3,0.));
#18158=CARTESIAN_POINT('',(-0.5,0.15,0.));
#18159=CARTESIAN_POINT('',(-0.5,0.225,0.075));
#18160=CARTESIAN_POINT('',(-0.5,-0.15,0.));
#18161=CARTESIAN_POINT('',(-0.5,0.3,0.));
#18162=CARTESIAN_POINT('',(-0.5,-0.3,0.15));
#18163=CARTESIAN_POINT('',(-0.5,-0.075,-0.075));
#18164=CARTESIAN_POINT('',(-0.5,-0.3,0.25));
#18165=CARTESIAN_POINT('',(-0.5,-0.3,0.));
#18166=CARTESIAN_POINT('',(-0.5,-0.5,0.25));
#18167=CARTESIAN_POINT('',(-0.5,-0.29,0.25));
#18168=CARTESIAN_POINT('',(-0.5,-0.5,0.25));
#18169=CARTESIAN_POINT('Origin',(-0.5,-0.5,0.25));
#18170=CARTESIAN_POINT('',(0.5,-0.5,0.25));
#18171=CARTESIAN_POINT('',(-0.5,-0.5,0.25));
#18172=CARTESIAN_POINT('',(0.5,-0.5,0.25));
#18173=CARTESIAN_POINT('Origin',(0.,-0.395,0.25));
#18174=CARTESIAN_POINT('',(0.5,-0.3,0.25));
#18175=CARTESIAN_POINT('',(-0.25,-0.3,0.25));
#18176=CARTESIAN_POINT('',(0.5,-0.5,0.25));
#18177=CARTESIAN_POINT('Origin',(0.5,-0.3,0.));
#18178=CARTESIAN_POINT('',(0.5,-0.3,0.15));
#18179=CARTESIAN_POINT('',(0.5,-0.3,0.));
#18180=CARTESIAN_POINT('',(0.5,-0.15,0.));
#18181=CARTESIAN_POINT('',(0.5,-0.225,0.075));
#18182=CARTESIAN_POINT('',(0.5,0.15,0.));
#18183=CARTESIAN_POINT('',(0.5,-0.3,0.));
#18184=CARTESIAN_POINT('',(0.5,0.3,0.15));
#18185=CARTESIAN_POINT('',(0.5,0.075,-0.075));
#18186=CARTESIAN_POINT('',(0.5,0.3,0.));
#18187=CARTESIAN_POINT('Origin',(-0.5,-0.3,0.));
#18188=CARTESIAN_POINT('',(-0.25,-0.3,0.15));
#18189=CARTESIAN_POINT('Origin',(-0.25,-0.225,0.075));
#18190=CARTESIAN_POINT('',(-0.149388386429468,-0.15,0.));
#18191=CARTESIAN_POINT('',(-0.25,-0.15,0.));
#18192=CARTESIAN_POINT('',(0.149388386429468,-0.15,0.));
#18193=CARTESIAN_POINT('Origin',(0.,0.,-0.15));
#18194=CARTESIAN_POINT('',(-0.25,-0.15,0.));
#18195=CARTESIAN_POINT('Origin',(0.,0.,-0.1));
#18196=CARTESIAN_POINT('',(-0.2117,-2.59257727379495E-17,0.));
#18197=CARTESIAN_POINT('Origin',(0.,0.,0.));
#18198=CARTESIAN_POINT('',(-0.2117,-2.59257727379495E-17,-0.1));
#18199=CARTESIAN_POINT('',(-0.149388386429468,0.15,0.));
#18200=CARTESIAN_POINT('Origin',(0.,0.,0.));
#18201=CARTESIAN_POINT('',(0.149388386429468,0.15,0.));
#18202=CARTESIAN_POINT('Origin',(0.,0.,-0.15));
#18203=CARTESIAN_POINT('Origin',(0.,0.,0.));
#18204=CARTESIAN_POINT('Origin',(0.,0.,0.));
#18205=CARTESIAN_POINT('',(0.25,0.15,0.));
#18206=CARTESIAN_POINT('Origin',(0.,0.,0.));
#18207=CARTESIAN_POINT('',(0.25,0.15,0.));
#18208=CARTESIAN_POINT('Origin',(0.25,0.225,0.075));
#18209=CARTESIAN_POINT('',(0.25,0.3,0.15));
#18210=CARTESIAN_POINT('Origin',(0.5,0.3,0.));
#18211=CARTESIAN_POINT('',(0.,0.,0.));
#18212=CARTESIAN_POINT('Origin',(0.115470053837925,-0.5,-0.2));
#18213=CARTESIAN_POINT('',(0.23094010767585,-0.5,0.));
#18214=CARTESIAN_POINT('',(0.115470053837925,-0.5,-0.2));
#18215=CARTESIAN_POINT('',(0.23094010767585,-0.5,0.));
#18216=CARTESIAN_POINT('',(0.115470053837925,-0.8,-0.2));
#18217=CARTESIAN_POINT('',(0.115470053837925,-0.5,-0.2));
#18218=CARTESIAN_POINT('',(0.23094010767585,-0.8,0.));
#18219=CARTESIAN_POINT('',(0.23094010767585,-0.8,0.));
#18220=CARTESIAN_POINT('',(0.23094010767585,-0.5,0.));
#18221=CARTESIAN_POINT('Origin',(-0.115470053837925,-0.5,-0.2));
#18222=CARTESIAN_POINT('',(-0.115470053837925,-0.5,-0.2));
#18223=CARTESIAN_POINT('',(0.115470053837925,-0.5,-0.2));
#18224=CARTESIAN_POINT('',(-0.115470053837925,-0.8,-0.2));
#18225=CARTESIAN_POINT('',(-0.115470053837925,-0.5,-0.2));
#18226=CARTESIAN_POINT('',(0.115470053837925,-0.8,-0.2));
#18227=CARTESIAN_POINT('Origin',(-0.23094010767585,-0.5,-2.77555756156289E-17));
#18228=CARTESIAN_POINT('',(-0.23094010767585,-0.5,-2.82820063659975E-17));
#18229=CARTESIAN_POINT('',(-0.115470053837925,-0.5,-0.2));
#18230=CARTESIAN_POINT('',(-0.23094010767585,-0.8,-2.77555756156289E-17));
#18231=CARTESIAN_POINT('',(-0.23094010767585,-0.5,-2.82820063659975E-17));
#18232=CARTESIAN_POINT('',(-0.115470053837925,-0.8,-0.2));
#18233=CARTESIAN_POINT('Origin',(-0.115470053837925,-0.5,0.2));
#18234=CARTESIAN_POINT('',(-0.115470053837925,-0.5,0.2));
#18235=CARTESIAN_POINT('',(-0.23094010767585,-0.5,-2.82820063659975E-17));
#18236=CARTESIAN_POINT('',(-0.115470053837925,-0.8,0.2));
#18237=CARTESIAN_POINT('',(-0.115470053837925,-0.5,0.2));
#18238=CARTESIAN_POINT('',(-0.23094010767585,-0.8,-2.82820063659975E-17));
#18239=CARTESIAN_POINT('Origin',(0.115470053837925,-0.5,0.2));
#18240=CARTESIAN_POINT('',(0.115470053837925,-0.5,0.2));
#18241=CARTESIAN_POINT('',(-0.115470053837925,-0.5,0.2));
#18242=CARTESIAN_POINT('',(0.115470053837925,-0.8,0.2));
#18243=CARTESIAN_POINT('',(0.115470053837925,-0.5,0.2));
#18244=CARTESIAN_POINT('',(-0.115470053837925,-0.8,0.2));
#18245=CARTESIAN_POINT('Origin',(0.23094010767585,-0.5,0.));
#18246=CARTESIAN_POINT('',(0.115470053837925,-0.5,0.2));
#18247=CARTESIAN_POINT('',(0.115470053837925,-0.8,0.2));
#18248=CARTESIAN_POINT('Origin',(0.,-0.5,0.));
#18249=CARTESIAN_POINT('Origin',(0.,-0.8,0.));
#18250=CARTESIAN_POINT('Origin',(0.,-1.75,0.));
#18251=CARTESIAN_POINT('',(-0.24505,-1.75,3.00099698131059E-17));
#18252=CARTESIAN_POINT('Origin',(0.,-1.75,0.));
#18253=CARTESIAN_POINT('Origin',(0.375,0.5,0.));
#18254=CARTESIAN_POINT('',(-0.375,0.5,-4.59242549680257E-17));
#18255=CARTESIAN_POINT('Origin',(0.,0.5,0.));
#18256=CARTESIAN_POINT('Origin',(0.,0.475,0.));
#18257=CARTESIAN_POINT('',(-0.425,0.45,-5.20474889637625E-17));
#18258=CARTESIAN_POINT('Origin',(0.,0.45,0.));
#18259=CARTESIAN_POINT('',(-0.4,0.475,-4.89858719658941E-17));
#18260=CARTESIAN_POINT('Origin',(0.,0.24,0.));
#18261=CARTESIAN_POINT('',(-0.425,0.0299999999999998,-5.20474889637625E-17));
#18262=CARTESIAN_POINT('Origin',(0.,0.0299999999999998,0.));
#18263=CARTESIAN_POINT('',(-0.425,0.24,-5.20474889637625E-17));
#18264=CARTESIAN_POINT('Origin',(0.,0.0150000000000001,0.));
#18265=CARTESIAN_POINT('',(-0.395,4.85722573273506E-17,-4.83735485663204E-17));
#18266=CARTESIAN_POINT('Origin',(0.,0.,0.));
#18267=CARTESIAN_POINT('',(-0.41,0.0150000000000001,-5.02105187650415E-17));
#18268=CARTESIAN_POINT('Origin',(0.27,0.,0.));
#18269=CARTESIAN_POINT('',(-0.27,0.,-3.30654635769785E-17));
#18270=CARTESIAN_POINT('Origin',(0.,0.,0.));
#18271=CARTESIAN_POINT('Origin',(0.,-0.02,0.));
#18272=CARTESIAN_POINT('',(-0.24505,-0.0498999999999999,3.00099698131059E-17));
#18273=CARTESIAN_POINT('Origin',(0.,-0.0498999999999999,0.));
#18274=CARTESIAN_POINT('',(-0.26,-0.02,-3.18408167778312E-17));
#18275=CARTESIAN_POINT('Origin',(0.,-0.995,0.));
#18276=CARTESIAN_POINT('',(-0.24505,-0.995,-3.00099698131059E-17));
#18277=CARTESIAN_POINT('',(0.,0.,0.));
#18278=CARTESIAN_POINT('Origin',(14.,0.,0.97));
#18279=CARTESIAN_POINT('',(13.625,-4.59242549680257E-17,0.97));
#18280=CARTESIAN_POINT('Origin',(14.,0.,0.97));
#18281=CARTESIAN_POINT('',(13.625,4.59242549680257E-17,1.5));
#18282=CARTESIAN_POINT('',(13.625,-4.59242549680257E-17,0.97));
#18283=CARTESIAN_POINT('Origin',(14.,0.,1.5));
#18284=CARTESIAN_POINT('Origin',(14.,0.,0.97));
#18285=CARTESIAN_POINT('',(13.775,-2.75545529808154E-17,0.97));
#18286=CARTESIAN_POINT('Origin',(14.,0.,0.97));
#18287=CARTESIAN_POINT('Origin',(8.,0.,0.97));
#18288=CARTESIAN_POINT('',(7.625,-4.59242549680257E-17,0.97));
#18289=CARTESIAN_POINT('Origin',(8.,0.,0.97));
#18290=CARTESIAN_POINT('',(7.625,4.59242549680257E-17,1.5));
#18291=CARTESIAN_POINT('',(7.625,-4.59242549680257E-17,0.97));
#18292=CARTESIAN_POINT('Origin',(8.,0.,1.5));
#18293=CARTESIAN_POINT('Origin',(8.,0.,0.97));
#18294=CARTESIAN_POINT('',(7.775,-2.75545529808154E-17,0.97));
#18295=CARTESIAN_POINT('Origin',(8.,0.,0.97));
#18296=CARTESIAN_POINT('Origin',(2.,0.,0.97));
#18297=CARTESIAN_POINT('',(1.625,-4.59242549680257E-17,0.97));
#18298=CARTESIAN_POINT('Origin',(2.,0.,0.97));
#18299=CARTESIAN_POINT('',(1.625,4.59242549680257E-17,1.5));
#18300=CARTESIAN_POINT('',(1.625,-4.59242549680257E-17,0.97));
#18301=CARTESIAN_POINT('Origin',(2.,0.,1.5));
#18302=CARTESIAN_POINT('Origin',(2.,0.,0.97));
#18303=CARTESIAN_POINT('',(1.775,-2.75545529808155E-17,0.97));
#18304=CARTESIAN_POINT('Origin',(2.,0.,0.97));
#18305=CARTESIAN_POINT('Origin',(20.,0.,0.97));
#18306=CARTESIAN_POINT('',(19.625,-4.59242549680257E-17,0.97));
#18307=CARTESIAN_POINT('Origin',(20.,0.,0.97));
#18308=CARTESIAN_POINT('',(19.625,4.59242549680257E-17,1.5));
#18309=CARTESIAN_POINT('',(19.625,-4.59242549680257E-17,0.97));
#18310=CARTESIAN_POINT('Origin',(20.,0.,1.5));
#18311=CARTESIAN_POINT('Origin',(20.,0.,0.97));
#18312=CARTESIAN_POINT('',(19.775,-2.75545529808156E-17,0.97));
#18313=CARTESIAN_POINT('Origin',(20.,0.,0.97));
#18314=CARTESIAN_POINT('Origin',(14.,0.,-0.1));
#18315=CARTESIAN_POINT('',(13.775,-2.75545529808154E-17,0.));
#18316=CARTESIAN_POINT('Origin',(14.,0.,0.));
#18317=CARTESIAN_POINT('',(13.775,-2.75545529808154E-17,-0.1));
#18318=CARTESIAN_POINT('Origin',(8.,0.,-0.1));
#18319=CARTESIAN_POINT('',(7.775,-2.75545529808154E-17,0.));
#18320=CARTESIAN_POINT('Origin',(8.,0.,0.));
#18321=CARTESIAN_POINT('',(7.775,-2.75545529808154E-17,-0.1));
#18322=CARTESIAN_POINT('Origin',(2.,0.,-0.1));
#18323=CARTESIAN_POINT('',(1.775,-2.75545529808155E-17,0.));
#18324=CARTESIAN_POINT('Origin',(2.,0.,0.));
#18325=CARTESIAN_POINT('',(1.775,-2.75545529808155E-17,-0.1));
#18326=CARTESIAN_POINT('Origin',(20.,0.,-0.1));
#18327=CARTESIAN_POINT('',(19.775,-2.75545529808156E-17,0.));
#18328=CARTESIAN_POINT('Origin',(20.,0.,0.));
#18329=CARTESIAN_POINT('',(19.775,-2.75545529808156E-17,-0.1));
#18330=CARTESIAN_POINT('Origin',(0.,-0.53,1.));
#18331=CARTESIAN_POINT('',(0.,-0.53,1.));
#18332=CARTESIAN_POINT('',(0.,-0.75,0.85));
#18333=CARTESIAN_POINT('',(0.,-0.53,1.));
#18334=CARTESIAN_POINT('',(22.,-0.75,0.85));
#18335=CARTESIAN_POINT('',(0.,-0.75,0.85));
#18336=CARTESIAN_POINT('',(22.,-0.53,1.));
#18337=CARTESIAN_POINT('',(22.,-0.53,1.));
#18338=CARTESIAN_POINT('',(0.,-0.53,1.));
#18339=CARTESIAN_POINT('Origin',(0.,-0.53,1.15));
#18340=CARTESIAN_POINT('',(0.,-0.53,1.15));
#18341=CARTESIAN_POINT('',(0.,-0.53,1.15));
#18342=CARTESIAN_POINT('',(22.,-0.53,1.15));
#18343=CARTESIAN_POINT('',(22.,-0.53,1.15));
#18344=CARTESIAN_POINT('',(0.,-0.53,1.15));
#18345=CARTESIAN_POINT('Origin',(0.,-0.75,1.3));
#18346=CARTESIAN_POINT('',(0.,-0.75,1.3));
#18347=CARTESIAN_POINT('',(0.,-0.75,1.3));
#18348=CARTESIAN_POINT('',(22.,-0.75,1.3));
#18349=CARTESIAN_POINT('',(22.,-0.75,1.3));
#18350=CARTESIAN_POINT('',(0.,-0.75,1.3));
#18351=CARTESIAN_POINT('Origin',(0.,-0.75,1.5));
#18352=CARTESIAN_POINT('',(0.,-0.75,1.5));
#18353=CARTESIAN_POINT('',(0.,-0.75,1.5));
#18354=CARTESIAN_POINT('',(22.,-0.75,1.5));
#18355=CARTESIAN_POINT('',(22.,-0.75,1.5));
#18356=CARTESIAN_POINT('',(0.,-0.75,1.5));
#18357=CARTESIAN_POINT('Origin',(0.,0.75,1.5));
#18358=CARTESIAN_POINT('',(0.,0.75,1.5));
#18359=CARTESIAN_POINT('',(0.,0.75,1.5));
#18360=CARTESIAN_POINT('',(22.,0.75,1.5));
#18361=CARTESIAN_POINT('',(22.,0.75,1.5));
#18362=CARTESIAN_POINT('',(0.,0.75,1.5));
#18363=CARTESIAN_POINT('Origin',(0.,0.75,1.3));
#18364=CARTESIAN_POINT('',(0.,0.75,1.3));
#18365=CARTESIAN_POINT('',(0.,0.75,1.3));
#18366=CARTESIAN_POINT('',(22.,0.75,1.3));
#18367=CARTESIAN_POINT('',(22.,0.75,1.3));
#18368=CARTESIAN_POINT('',(0.,0.75,1.3));
#18369=CARTESIAN_POINT('Origin',(0.,0.53,1.15));
#18370=CARTESIAN_POINT('',(0.,0.53,1.15));
#18371=CARTESIAN_POINT('',(0.,0.53,1.15));
#18372=CARTESIAN_POINT('',(22.,0.53,1.15));
#18373=CARTESIAN_POINT('',(22.,0.53,1.15));
#18374=CARTESIAN_POINT('',(0.,0.53,1.15));
#18375=CARTESIAN_POINT('Origin',(0.,0.53,1.));
#18376=CARTESIAN_POINT('',(0.,0.53,1.));
#18377=CARTESIAN_POINT('',(0.,0.53,1.));
#18378=CARTESIAN_POINT('',(22.,0.53,1.));
#18379=CARTESIAN_POINT('',(22.,0.53,1.));
#18380=CARTESIAN_POINT('',(0.,0.53,1.));
#18381=CARTESIAN_POINT('Origin',(0.,0.75,0.85));
#18382=CARTESIAN_POINT('',(0.,0.75,0.85));
#18383=CARTESIAN_POINT('',(0.,0.75,0.85));
#18384=CARTESIAN_POINT('',(22.,0.75,0.85));
#18385=CARTESIAN_POINT('',(22.,0.75,0.85));
#18386=CARTESIAN_POINT('',(0.,0.75,0.85));
#18387=CARTESIAN_POINT('Origin',(0.,0.75,0.));
#18388=CARTESIAN_POINT('',(0.,0.75,0.));
#18389=CARTESIAN_POINT('',(0.,0.75,0.));
#18390=CARTESIAN_POINT('',(22.,0.75,0.));
#18391=CARTESIAN_POINT('',(22.,0.75,0.));
#18392=CARTESIAN_POINT('',(0.,0.75,0.));
#18393=CARTESIAN_POINT('Origin',(0.,-0.75,0.));
#18394=CARTESIAN_POINT('',(0.,-0.75,0.));
#18395=CARTESIAN_POINT('',(0.,-0.75,0.));
#18396=CARTESIAN_POINT('',(22.,-0.75,0.));
#18397=CARTESIAN_POINT('',(22.,-0.75,0.));
#18398=CARTESIAN_POINT('',(0.,-0.75,0.));
#18399=CARTESIAN_POINT('Origin',(0.,-0.75,0.85));
#18400=CARTESIAN_POINT('',(0.,-0.75,0.85));
#18401=CARTESIAN_POINT('',(22.,-0.75,0.85));
#18402=CARTESIAN_POINT('Origin',(22.,0.,0.75));
#18403=CARTESIAN_POINT('Origin',(0.,0.,0.75));
#18404=CARTESIAN_POINT('',(0.,0.,0.));
#18405=CARTESIAN_POINT('',(0.,0.,0.));
#18406=CARTESIAN_POINT('Origin',(0.,-5.1,7.));
#18407=CARTESIAN_POINT('',(-0.165,-5.,7.));
#18408=CARTESIAN_POINT('Origin',(0.,-5.,7.));
#18409=CARTESIAN_POINT('',(-0.165,-3.4,7.));
#18410=CARTESIAN_POINT('',(-0.165,-5.1,7.));
#18411=CARTESIAN_POINT('Origin',(0.,-3.4,7.));
#18412=CARTESIAN_POINT('Origin',(0.,-3.4,7.));
#18413=CARTESIAN_POINT('Origin',(0.,2.05,7.));
#18414=CARTESIAN_POINT('',(-0.7,2.05,7.));
#18415=CARTESIAN_POINT('Origin',(0.,2.05,7.));
#18416=CARTESIAN_POINT('',(-0.5,2.05,7.));
#18417=CARTESIAN_POINT('Origin',(0.,2.05,7.));
#18418=CARTESIAN_POINT('Origin',(0.,1.35,7.));
#18419=CARTESIAN_POINT('',(-0.7,1.35,7.));
#18420=CARTESIAN_POINT('Origin',(0.,1.35,7.));
#18421=CARTESIAN_POINT('',(-0.5,1.35,7.));
#18422=CARTESIAN_POINT('Origin',(0.,1.35,7.));
#18423=CARTESIAN_POINT('Origin',(0.,1.35,7.));
#18424=CARTESIAN_POINT('',(-0.7,1.35,7.));
#18425=CARTESIAN_POINT('Origin',(0.,-1.8,7.));
#18426=CARTESIAN_POINT('',(-0.5,-1.8,7.));
#18427=CARTESIAN_POINT('',(-0.5,-1.8,7.));
#18428=CARTESIAN_POINT('Origin',(0.,-1.8,7.));
#18429=CARTESIAN_POINT('Origin',(0.,-5.,7.));
#18430=CARTESIAN_POINT('',(-0.4,-1.8,7.));
#18431=CARTESIAN_POINT('Origin',(0.,-1.8,7.));
#18432=CARTESIAN_POINT('',(-0.4,-5.,7.));
#18433=CARTESIAN_POINT('',(-0.4,-5.,7.));
#18434=CARTESIAN_POINT('Origin',(0.,-5.,7.));
#18435=CARTESIAN_POINT('Origin',(0.,-5.,7.));
#18436=CARTESIAN_POINT('Origin',(0.,-1.8,7.));
#18437=CARTESIAN_POINT('',(-0.5,3.,7.));
#18438=CARTESIAN_POINT('Origin',(0.,3.,7.));
#18439=CARTESIAN_POINT('',(-0.5,-1.8,7.));
#18440=CARTESIAN_POINT('Origin',(0.,3.,7.));
#18441=CARTESIAN_POINT('Origin',(0.,-1.8,7.));
#18442=CARTESIAN_POINT('',(0.,0.,0.));
#18443=CARTESIAN_POINT('Origin',(0.,-1.8,7.));
#18444=CARTESIAN_POINT('',(-0.505,-1.8,7.));
#18445=CARTESIAN_POINT('Origin',(0.,-1.8,7.));
#18446=CARTESIAN_POINT('',(-0.505,-1.35,7.));
#18447=CARTESIAN_POINT('',(-0.505,-1.8,7.));
#18448=CARTESIAN_POINT('Origin',(0.,-1.35,7.));
#18449=CARTESIAN_POINT('Origin',(0.,-1.8,7.));
#18450=CARTESIAN_POINT('',(-0.405,-1.8,7.));
#18451=CARTESIAN_POINT('Origin',(0.,-1.8,7.));
#18452=CARTESIAN_POINT('Origin',(0.,-2.65,7.));
#18453=CARTESIAN_POINT('',(-0.405,-2.65,7.));
#18454=CARTESIAN_POINT('',(-0.405,-2.65,7.));
#18455=CARTESIAN_POINT('Origin',(0.,-2.65,7.));
#18456=CARTESIAN_POINT('Origin',(0.,-2.65,7.));
#18457=CARTESIAN_POINT('',(-0.7,-1.35,7.));
#18458=CARTESIAN_POINT('Origin',(0.,-1.35,7.));
#18459=CARTESIAN_POINT('',(-0.7,-2.65,7.));
#18460=CARTESIAN_POINT('',(-0.7,-2.65,7.));
#18461=CARTESIAN_POINT('Origin',(0.,-2.65,7.));
#18462=CARTESIAN_POINT('Origin',(0.,-1.35,7.));
#18463=CARTESIAN_POINT('Origin',(0.,-2.65,7.));
#18464=CARTESIAN_POINT('',(0.,0.,0.));
#18465=CARTESIAN_POINT('Origin',(0.,-0.45,7.));
#18466=CARTESIAN_POINT('',(-0.505,0.45,7.));
#18467=CARTESIAN_POINT('Origin',(0.,0.45,7.));
#18468=CARTESIAN_POINT('',(-0.505,-0.45,7.));
#18469=CARTESIAN_POINT('',(-0.505,-0.45,7.));
#18470=CARTESIAN_POINT('Origin',(0.,-0.45,7.));
#18471=CARTESIAN_POINT('Origin',(0.,-0.45,7.));
#18472=CARTESIAN_POINT('',(-0.7,0.45,7.));
#18473=CARTESIAN_POINT('Origin',(0.,0.45,7.));
#18474=CARTESIAN_POINT('',(-0.7,-0.45,7.));
#18475=CARTESIAN_POINT('',(-0.7,-0.45,7.));
#18476=CARTESIAN_POINT('Origin',(0.,-0.45,7.));
#18477=CARTESIAN_POINT('Origin',(0.,0.45,7.));
#18478=CARTESIAN_POINT('Origin',(0.,-0.45,7.));
#18479=CARTESIAN_POINT('',(0.,0.,0.));
#18480=CARTESIAN_POINT('Origin',(0.,-3.95,6.35));
#18481=CARTESIAN_POINT('',(-0.15,-3.95,6.6));
#18482=CARTESIAN_POINT('Origin',(0.,-3.95,6.6));
#18483=CARTESIAN_POINT('',(-0.15,-3.95,6.35));
#18484=CARTESIAN_POINT('',(-0.15,-3.95,6.35));
#18485=CARTESIAN_POINT('Origin',(0.,-3.95,6.35));
#18486=CARTESIAN_POINT('Origin',(0.,-3.95,6.6));
#18487=CARTESIAN_POINT('Origin',(0.,-3.95,6.35));
#18488=CARTESIAN_POINT('',(0.,0.,0.));
#18489=CARTESIAN_POINT('Origin',(0.,-3.95,7.4));
#18490=CARTESIAN_POINT('',(-0.15,-3.95,7.65));
#18491=CARTESIAN_POINT('Origin',(0.,-3.95,7.65));
#18492=CARTESIAN_POINT('',(-0.15,-3.95,7.4));
#18493=CARTESIAN_POINT('',(-0.15,-3.95,7.4));
#18494=CARTESIAN_POINT('Origin',(0.,-3.95,7.4));
#18495=CARTESIAN_POINT('Origin',(0.,-3.95,7.65));
#18496=CARTESIAN_POINT('Origin',(0.,-3.95,7.4));
#18497=CARTESIAN_POINT('',(0.,0.,0.));
#18498=CARTESIAN_POINT('Origin',(0.,-5.2,7.));
#18499=CARTESIAN_POINT('',(-0.225,-5.,7.));
#18500=CARTESIAN_POINT('Origin',(0.,-5.,7.));
#18501=CARTESIAN_POINT('',(-0.225,-5.2,7.));
#18502=CARTESIAN_POINT('',(-0.225,-5.2,7.));
#18503=CARTESIAN_POINT('Origin',(0.,-5.2,7.));
#18504=CARTESIAN_POINT('Origin',(0.,-5.2,7.));
#18505=CARTESIAN_POINT('',(-0.6,-5.,7.));
#18506=CARTESIAN_POINT('Origin',(0.,-5.,7.));
#18507=CARTESIAN_POINT('',(-0.6,-5.2,7.));
#18508=CARTESIAN_POINT('',(-0.6,-5.2,7.));
#18509=CARTESIAN_POINT('Origin',(0.,-5.2,7.));
#18510=CARTESIAN_POINT('Origin',(0.,-5.,7.));
#18511=CARTESIAN_POINT('Origin',(0.,-5.2,7.));
#18512=CARTESIAN_POINT('',(0.,0.,0.));
#18513=CARTESIAN_POINT('',(0.,0.,0.));
#18514=CARTESIAN_POINT('Origin',(32.,-5.1,7.));
#18515=CARTESIAN_POINT('',(31.835,-5.,7.));
#18516=CARTESIAN_POINT('Origin',(32.,-5.,7.));
#18517=CARTESIAN_POINT('',(31.835,-3.4,7.));
#18518=CARTESIAN_POINT('',(31.835,-5.1,7.));
#18519=CARTESIAN_POINT('Origin',(32.,-3.4,7.));
#18520=CARTESIAN_POINT('Origin',(32.,-3.4,7.));
#18521=CARTESIAN_POINT('Origin',(32.,2.05,7.));
#18522=CARTESIAN_POINT('',(31.3,2.05,7.));
#18523=CARTESIAN_POINT('Origin',(32.,2.05,7.));
#18524=CARTESIAN_POINT('',(31.5,2.05,7.));
#18525=CARTESIAN_POINT('Origin',(32.,2.05,7.));
#18526=CARTESIAN_POINT('Origin',(32.,1.35,7.));
#18527=CARTESIAN_POINT('',(31.3,1.35,7.));
#18528=CARTESIAN_POINT('Origin',(32.,1.35,7.));
#18529=CARTESIAN_POINT('',(31.5,1.35,7.));
#18530=CARTESIAN_POINT('Origin',(32.,1.35,7.));
#18531=CARTESIAN_POINT('Origin',(32.,1.35,7.));
#18532=CARTESIAN_POINT('',(31.3,1.35,7.));
#18533=CARTESIAN_POINT('Origin',(32.,-1.8,7.));
#18534=CARTESIAN_POINT('',(31.5,-1.8,7.));
#18535=CARTESIAN_POINT('',(31.5,-1.8,7.));
#18536=CARTESIAN_POINT('Origin',(32.,-1.8,7.));
#18537=CARTESIAN_POINT('Origin',(32.,-5.,7.));
#18538=CARTESIAN_POINT('',(31.6,-1.8,7.));
#18539=CARTESIAN_POINT('Origin',(32.,-1.8,7.));
#18540=CARTESIAN_POINT('',(31.6,-5.,7.));
#18541=CARTESIAN_POINT('',(31.6,-5.,7.));
#18542=CARTESIAN_POINT('Origin',(32.,-5.,7.));
#18543=CARTESIAN_POINT('Origin',(32.,-5.,7.));
#18544=CARTESIAN_POINT('Origin',(32.,-1.8,7.));
#18545=CARTESIAN_POINT('',(31.5,3.,7.));
#18546=CARTESIAN_POINT('Origin',(32.,3.,7.));
#18547=CARTESIAN_POINT('',(31.5,-1.8,7.));
#18548=CARTESIAN_POINT('Origin',(32.,3.,7.));
#18549=CARTESIAN_POINT('Origin',(32.,-1.8,7.));
#18550=CARTESIAN_POINT('',(0.,0.,0.));
#18551=CARTESIAN_POINT('Origin',(32.,-1.8,7.));
#18552=CARTESIAN_POINT('',(31.495,-1.8,7.));
#18553=CARTESIAN_POINT('Origin',(32.,-1.8,7.));
#18554=CARTESIAN_POINT('',(31.495,-1.35,7.));
#18555=CARTESIAN_POINT('',(31.495,-1.8,7.));
#18556=CARTESIAN_POINT('Origin',(32.,-1.35,7.));
#18557=CARTESIAN_POINT('Origin',(32.,-1.8,7.));
#18558=CARTESIAN_POINT('',(31.595,-1.8,7.));
#18559=CARTESIAN_POINT('Origin',(32.,-1.8,7.));
#18560=CARTESIAN_POINT('Origin',(32.,-2.65,7.));
#18561=CARTESIAN_POINT('',(31.595,-2.65,7.));
#18562=CARTESIAN_POINT('',(31.595,-2.65,7.));
#18563=CARTESIAN_POINT('Origin',(32.,-2.65,7.));
#18564=CARTESIAN_POINT('Origin',(32.,-2.65,7.));
#18565=CARTESIAN_POINT('',(31.3,-1.35,7.));
#18566=CARTESIAN_POINT('Origin',(32.,-1.35,7.));
#18567=CARTESIAN_POINT('',(31.3,-2.65,7.));
#18568=CARTESIAN_POINT('',(31.3,-2.65,7.));
#18569=CARTESIAN_POINT('Origin',(32.,-2.65,7.));
#18570=CARTESIAN_POINT('Origin',(32.,-1.35,7.));
#18571=CARTESIAN_POINT('Origin',(32.,-2.65,7.));
#18572=CARTESIAN_POINT('',(0.,0.,0.));
#18573=CARTESIAN_POINT('Origin',(32.,-0.45,7.));
#18574=CARTESIAN_POINT('',(31.495,0.45,7.));
#18575=CARTESIAN_POINT('Origin',(32.,0.45,7.));
#18576=CARTESIAN_POINT('',(31.495,-0.45,7.));
#18577=CARTESIAN_POINT('',(31.495,-0.45,7.));
#18578=CARTESIAN_POINT('Origin',(32.,-0.45,7.));
#18579=CARTESIAN_POINT('Origin',(32.,-0.45,7.));
#18580=CARTESIAN_POINT('',(31.3,0.45,7.));
#18581=CARTESIAN_POINT('Origin',(32.,0.45,7.));
#18582=CARTESIAN_POINT('',(31.3,-0.45,7.));
#18583=CARTESIAN_POINT('',(31.3,-0.45,7.));
#18584=CARTESIAN_POINT('Origin',(32.,-0.45,7.));
#18585=CARTESIAN_POINT('Origin',(32.,0.45,7.));
#18586=CARTESIAN_POINT('Origin',(32.,-0.45,7.));
#18587=CARTESIAN_POINT('',(0.,0.,0.));
#18588=CARTESIAN_POINT('Origin',(32.,-3.95,6.35));
#18589=CARTESIAN_POINT('',(31.85,-3.95,6.6));
#18590=CARTESIAN_POINT('Origin',(32.,-3.95,6.6));
#18591=CARTESIAN_POINT('',(31.85,-3.95,6.35));
#18592=CARTESIAN_POINT('',(31.85,-3.95,6.35));
#18593=CARTESIAN_POINT('Origin',(32.,-3.95,6.35));
#18594=CARTESIAN_POINT('Origin',(32.,-3.95,6.6));
#18595=CARTESIAN_POINT('Origin',(32.,-3.95,6.35));
#18596=CARTESIAN_POINT('',(0.,0.,0.));
#18597=CARTESIAN_POINT('Origin',(32.,-3.95,7.4));
#18598=CARTESIAN_POINT('',(31.85,-3.95,7.65));
#18599=CARTESIAN_POINT('Origin',(32.,-3.95,7.65));
#18600=CARTESIAN_POINT('',(31.85,-3.95,7.4));
#18601=CARTESIAN_POINT('',(31.85,-3.95,7.4));
#18602=CARTESIAN_POINT('Origin',(32.,-3.95,7.4));
#18603=CARTESIAN_POINT('Origin',(32.,-3.95,7.65));
#18604=CARTESIAN_POINT('Origin',(32.,-3.95,7.4));
#18605=CARTESIAN_POINT('',(0.,0.,0.));
#18606=CARTESIAN_POINT('Origin',(32.,-5.2,7.));
#18607=CARTESIAN_POINT('',(31.775,-5.,7.));
#18608=CARTESIAN_POINT('Origin',(32.,-5.,7.));
#18609=CARTESIAN_POINT('',(31.775,-5.2,7.));
#18610=CARTESIAN_POINT('',(31.775,-5.2,7.));
#18611=CARTESIAN_POINT('Origin',(32.,-5.2,7.));
#18612=CARTESIAN_POINT('Origin',(32.,-5.2,7.));
#18613=CARTESIAN_POINT('',(31.4,-5.,7.));
#18614=CARTESIAN_POINT('Origin',(32.,-5.,7.));
#18615=CARTESIAN_POINT('',(31.4,-5.2,7.));
#18616=CARTESIAN_POINT('',(31.4,-5.2,7.));
#18617=CARTESIAN_POINT('Origin',(32.,-5.2,7.));
#18618=CARTESIAN_POINT('Origin',(32.,-5.,7.));
#18619=CARTESIAN_POINT('Origin',(32.,-5.2,7.));
#18620=CARTESIAN_POINT('',(0.,0.,0.));
#18621=CARTESIAN_POINT('Origin',(0.,-0.45,0.));
#18622=CARTESIAN_POINT('',(-0.65,-0.325,-3.9801020972289E-17));
#18623=CARTESIAN_POINT('',(-0.637867541108654,-0.45,0.125));
#18624=CARTESIAN_POINT('Ctrl Pts',(-0.65,-0.325,-6.93889390390723E-17));
#18625=CARTESIAN_POINT('Ctrl Pts',(-0.65,-0.325,0.0157371373481997));
#18626=CARTESIAN_POINT('Ctrl Pts',(-0.649370620646074,-0.328153081062251,
0.0324967135411163));
#18627=CARTESIAN_POINT('Ctrl Pts',(-0.647096224417991,-0.340922081922822,
0.0632828231545122));
#18628=CARTESIAN_POINT('Ctrl Pts',(-0.645482573914132,-0.350535859112198,
0.0773125544088347));
#18629=CARTESIAN_POINT('Ctrl Pts',(-0.642442040715078,-0.372687974598127,
0.0994646698947638));
#18630=CARTESIAN_POINT('Ctrl Pts',(-0.640815160902589,-0.386717480603274,
0.109078032552995));
#18631=CARTESIAN_POINT('Ctrl Pts',(-0.63851034608138,-0.417502809542363,
0.121846732641678));
#18632=CARTESIAN_POINT('Ctrl Pts',(-0.637867541108654,-0.434262111007648,
0.125));
#18633=CARTESIAN_POINT('Ctrl Pts',(-0.637867541108654,-0.45,0.125));
#18634=CARTESIAN_POINT('',(-0.65,-0.575,-3.9801020972289E-17));
#18635=CARTESIAN_POINT('Ctrl Pts',(-0.65,-0.575,-3.46944695195361E-18));
#18636=CARTESIAN_POINT('Ctrl Pts',(-0.65,-0.575,-0.0157371373481998));
#18637=CARTESIAN_POINT('Ctrl Pts',(-0.649370620646074,-0.571846918937749,
-0.0324967135411164));
#18638=CARTESIAN_POINT('Ctrl Pts',(-0.647096224417991,-0.559077918077178,
-0.0632828231545123));
#18639=CARTESIAN_POINT('Ctrl Pts',(-0.645482573914132,-0.549464140887802,
-0.0773125544088349));
#18640=CARTESIAN_POINT('Ctrl Pts',(-0.642442040715078,-0.527312025401873,
-0.099464669894764));
#18641=CARTESIAN_POINT('Ctrl Pts',(-0.640815160902589,-0.513282519396725,
-0.109078032552995));
#18642=CARTESIAN_POINT('Ctrl Pts',(-0.63851034608138,-0.482497190457637,
-0.121846732641678));
#18643=CARTESIAN_POINT('Ctrl Pts',(-0.637867541108654,-0.465737888992352,
-0.125));
#18644=CARTESIAN_POINT('Ctrl Pts',(-0.637867541108654,-0.434262111007648,
-0.125));
#18645=CARTESIAN_POINT('Ctrl Pts',(-0.63851034608138,-0.417502809542363,
-0.121846732641678));
#18646=CARTESIAN_POINT('Ctrl Pts',(-0.640815160902589,-0.386717480603275,
-0.109078032552995));
#18647=CARTESIAN_POINT('Ctrl Pts',(-0.642442040715078,-0.372687974598127,
-0.099464669894764));
#18648=CARTESIAN_POINT('Ctrl Pts',(-0.645482573914132,-0.350535859112198,
-0.077312554408835));
#18649=CARTESIAN_POINT('Ctrl Pts',(-0.647096224417991,-0.340922081922822,
-0.0632828231545124));
#18650=CARTESIAN_POINT('Ctrl Pts',(-0.649370620646074,-0.328153081062251,
-0.0324967135411165));
#18651=CARTESIAN_POINT('Ctrl Pts',(-0.65,-0.325,-0.0157371373481999));
#18652=CARTESIAN_POINT('Ctrl Pts',(-0.65,-0.325,-8.32667268468867E-17));
#18653=CARTESIAN_POINT('Ctrl Pts',(-0.637867541108654,-0.45,0.125));
#18654=CARTESIAN_POINT('Ctrl Pts',(-0.637867541108654,-0.465737888992352,
0.125));
#18655=CARTESIAN_POINT('Ctrl Pts',(-0.63851034608138,-0.482497190457637,
0.121846732641678));
#18656=CARTESIAN_POINT('Ctrl Pts',(-0.640815160902589,-0.513282519396725,
0.109078032552995));
#18657=CARTESIAN_POINT('Ctrl Pts',(-0.642442040715078,-0.527312025401873,
0.0994646698947639));
#18658=CARTESIAN_POINT('Ctrl Pts',(-0.645482573914132,-0.549464140887802,
0.0773125544088349));
#18659=CARTESIAN_POINT('Ctrl Pts',(-0.647096224417991,-0.559077918077178,
0.0632828231545123));
#18660=CARTESIAN_POINT('Ctrl Pts',(-0.649370620646074,-0.571846918937749,
0.0324967135411164));
#18661=CARTESIAN_POINT('Ctrl Pts',(-0.65,-0.575,0.0157371373481998));
#18662=CARTESIAN_POINT('Ctrl Pts',(-0.65,-0.575,-2.08166817117217E-17));
#18663=CARTESIAN_POINT('',(-0.379967103839267,-0.45,0.125));
#18664=CARTESIAN_POINT('',(-7.65404249467096E-18,-0.45,0.125));
#18665=CARTESIAN_POINT('',(-0.4,-0.575,5.41097774720219E-18));
#18666=CARTESIAN_POINT('Ctrl Pts',(-0.4,-0.575,-3.81639164714898E-17));
#18667=CARTESIAN_POINT('Ctrl Pts',(-0.4,-0.575,0.0158075115832675));
#18668=CARTESIAN_POINT('Ctrl Pts',(-0.398970551469948,-0.571819306519379,
0.0325978607437828));
#18669=CARTESIAN_POINT('Ctrl Pts',(-0.395252954914593,-0.559029081159106,
0.0633657881355917));
#18670=CARTESIAN_POINT('Ctrl Pts',(-0.392612801026882,-0.549425200318011,
0.0773514949786256));
#18671=CARTESIAN_POINT('Ctrl Pts',(-0.38761064154154,-0.527347592689753,
0.0994291026068839));
#18672=CARTESIAN_POINT('Ctrl Pts',(-0.384911758361269,-0.51336346023721,
0.109029967924066));
#18673=CARTESIAN_POINT('Ctrl Pts',(-0.381057715344782,-0.48260129709332,
0.121817958968287));
#18674=CARTESIAN_POINT('Ctrl Pts',(-0.379967103839267,-0.465813100629203,
0.125));
#18675=CARTESIAN_POINT('Ctrl Pts',(-0.379967103839267,-0.45,0.125));
#18676=CARTESIAN_POINT('',(-0.379967103839267,-0.45,-0.125));
#18677=CARTESIAN_POINT('Ctrl Pts',(-0.379967103839267,-0.45,-0.125));
#18678=CARTESIAN_POINT('Ctrl Pts',(-0.379967103839267,-0.465813100629203,
-0.125));
#18679=CARTESIAN_POINT('Ctrl Pts',(-0.381057715344782,-0.48260129709332,
-0.121817958968287));
#18680=CARTESIAN_POINT('Ctrl Pts',(-0.384911758361269,-0.51336346023721,
-0.109029967924066));
#18681=CARTESIAN_POINT('Ctrl Pts',(-0.38761064154154,-0.527347592689753,
-0.099429102606884));
#18682=CARTESIAN_POINT('Ctrl Pts',(-0.392612801026882,-0.549425200318011,
-0.0773514949786257));
#18683=CARTESIAN_POINT('Ctrl Pts',(-0.395252954914593,-0.559029081159106,
-0.0633657881355918));
#18684=CARTESIAN_POINT('Ctrl Pts',(-0.398970551469948,-0.571819306519379,
-0.0325978607437828));
#18685=CARTESIAN_POINT('Ctrl Pts',(-0.4,-0.575,-0.0158075115832676));
#18686=CARTESIAN_POINT('Ctrl Pts',(-0.4,-0.575,-4.16333634234434E-17));
#18687=CARTESIAN_POINT('',(-0.4,-0.325,2.96971064108775E-17));
#18688=CARTESIAN_POINT('Ctrl Pts',(-0.4,-0.325,1.04083408558608E-17));
#18689=CARTESIAN_POINT('Ctrl Pts',(-0.4,-0.325,-0.0158075115832676));
#18690=CARTESIAN_POINT('Ctrl Pts',(-0.398970551469948,-0.328180693480621,
-0.0325978607437828));
#18691=CARTESIAN_POINT('Ctrl Pts',(-0.395252954914593,-0.340970918840894,
-0.0633657881355918));
#18692=CARTESIAN_POINT('Ctrl Pts',(-0.392612801026882,-0.350574799681989,
-0.0773514949786256));
#18693=CARTESIAN_POINT('Ctrl Pts',(-0.38761064154154,-0.372652407310247,
-0.0994291026068839));
#18694=CARTESIAN_POINT('Ctrl Pts',(-0.384911758361269,-0.38663653976279,
-0.109029967924066));
#18695=CARTESIAN_POINT('Ctrl Pts',(-0.381057715344782,-0.41739870290668,
-0.121817958968287));
#18696=CARTESIAN_POINT('Ctrl Pts',(-0.379967103839267,-0.434186899370797,
-0.125));
#18697=CARTESIAN_POINT('Ctrl Pts',(-0.379967103839267,-0.45,-0.125));
#18698=CARTESIAN_POINT('Ctrl Pts',(-0.379967103839267,-0.45,0.125));
#18699=CARTESIAN_POINT('Ctrl Pts',(-0.379967103839267,-0.434186899370797,
0.125));
#18700=CARTESIAN_POINT('Ctrl Pts',(-0.381057715344782,-0.41739870290668,
0.121817958968287));
#18701=CARTESIAN_POINT('Ctrl Pts',(-0.384911758361269,-0.38663653976279,
0.109029967924066));
#18702=CARTESIAN_POINT('Ctrl Pts',(-0.38761064154154,-0.372652407310247,
0.0994291026068839));
#18703=CARTESIAN_POINT('Ctrl Pts',(-0.392612801026882,-0.350574799681989,
0.0773514949786257));
#18704=CARTESIAN_POINT('Ctrl Pts',(-0.395252954914593,-0.340970918840894,
0.0633657881355918));
#18705=CARTESIAN_POINT('Ctrl Pts',(-0.398970551469948,-0.328180693480621,
0.0325978607437829));
#18706=CARTESIAN_POINT('Ctrl Pts',(-0.4,-0.325,0.0158075115832676));
#18707=CARTESIAN_POINT('Ctrl Pts',(-0.4,-0.325,1.38777878078145E-17));
#18708=CARTESIAN_POINT('Origin',(0.,-0.45,0.));
#18709=CARTESIAN_POINT('',(0.379967103839267,-0.45,-0.125));
#18710=CARTESIAN_POINT('',(0.379967103839267,-0.45,0.125));
#18711=CARTESIAN_POINT('Ctrl Pts',(0.379967103839267,-0.45,-0.125));
#18712=CARTESIAN_POINT('Ctrl Pts',(0.379967103839267,-0.434186899370797,
-0.125));
#18713=CARTESIAN_POINT('Ctrl Pts',(0.381057715344782,-0.41739870290668,
-0.121817958968287));
#18714=CARTESIAN_POINT('Ctrl Pts',(0.384911758361269,-0.38663653976279,
-0.109029967924066));
#18715=CARTESIAN_POINT('Ctrl Pts',(0.38761064154154,-0.372652407310247,
-0.0994291026068839));
#18716=CARTESIAN_POINT('Ctrl Pts',(0.392612801026882,-0.350574799681989,
-0.0773514949786256));
#18717=CARTESIAN_POINT('Ctrl Pts',(0.395252954914593,-0.340970918840894,
-0.0633657881355917));
#18718=CARTESIAN_POINT('Ctrl Pts',(0.398970551469948,-0.328180693480621,
-0.0325978607437828));
#18719=CARTESIAN_POINT('Ctrl Pts',(0.4,-0.325,-0.0158075115832675));
#18720=CARTESIAN_POINT('Ctrl Pts',(0.4,-0.325,0.0158075115832676));
#18721=CARTESIAN_POINT('Ctrl Pts',(0.398970551469948,-0.328180693480621,
0.0325978607437829));
#18722=CARTESIAN_POINT('Ctrl Pts',(0.395252954914593,-0.340970918840894,
0.0633657881355918));
#18723=CARTESIAN_POINT('Ctrl Pts',(0.392612801026882,-0.350574799681989,
0.0773514949786257));
#18724=CARTESIAN_POINT('Ctrl Pts',(0.38761064154154,-0.372652407310247,
0.099429102606884));
#18725=CARTESIAN_POINT('Ctrl Pts',(0.384911758361269,-0.38663653976279,
0.109029967924066));
#18726=CARTESIAN_POINT('Ctrl Pts',(0.381057715344782,-0.41739870290668,
0.121817958968287));
#18727=CARTESIAN_POINT('Ctrl Pts',(0.379967103839267,-0.434186899370797,
0.125));
#18728=CARTESIAN_POINT('Ctrl Pts',(0.379967103839267,-0.45,0.125));
#18729=CARTESIAN_POINT('Ctrl Pts',(0.379967103839267,-0.45,0.125));
#18730=CARTESIAN_POINT('Ctrl Pts',(0.379967103839267,-0.465813100629203,
0.125));
#18731=CARTESIAN_POINT('Ctrl Pts',(0.381057715344782,-0.48260129709332,
0.121817958968287));
#18732=CARTESIAN_POINT('Ctrl Pts',(0.384911758361269,-0.51336346023721,
0.109029967924066));
#18733=CARTESIAN_POINT('Ctrl Pts',(0.38761064154154,-0.527347592689753,
0.0994291026068839));
#18734=CARTESIAN_POINT('Ctrl Pts',(0.392612801026882,-0.549425200318011,
0.0773514949786257));
#18735=CARTESIAN_POINT('Ctrl Pts',(0.395252954914593,-0.559029081159106,
0.0633657881355918));
#18736=CARTESIAN_POINT('Ctrl Pts',(0.398970551469948,-0.571819306519379,
0.0325978607437829));
#18737=CARTESIAN_POINT('Ctrl Pts',(0.4,-0.575,0.0158075115832676));
#18738=CARTESIAN_POINT('Ctrl Pts',(0.4,-0.575,-0.0158075115832676));
#18739=CARTESIAN_POINT('Ctrl Pts',(0.398970551469948,-0.57181930651938,
-0.0325978607437828));
#18740=CARTESIAN_POINT('Ctrl Pts',(0.395252954914593,-0.559029081159106,
-0.0633657881355918));
#18741=CARTESIAN_POINT('Ctrl Pts',(0.392612801026882,-0.549425200318011,
-0.0773514949786257));
#18742=CARTESIAN_POINT('Ctrl Pts',(0.38761064154154,-0.527347592689753,
-0.0994291026068839));
#18743=CARTESIAN_POINT('Ctrl Pts',(0.384911758361269,-0.51336346023721,
-0.109029967924066));
#18744=CARTESIAN_POINT('Ctrl Pts',(0.381057715344782,-0.48260129709332,
-0.121817958968287));
#18745=CARTESIAN_POINT('Ctrl Pts',(0.379967103839267,-0.465813100629203,
-0.125));
#18746=CARTESIAN_POINT('Ctrl Pts',(0.379967103839267,-0.45,-0.125));
#18747=CARTESIAN_POINT('',(0.637867541108654,-0.45,0.125));
#18748=CARTESIAN_POINT('',(-7.65404249467096E-18,-0.45,0.125));
#18749=CARTESIAN_POINT('',(0.65,-0.575,3.9801020972289E-17));
#18750=CARTESIAN_POINT('Ctrl Pts',(0.65,-0.575,5.55111512312578E-17));
#18751=CARTESIAN_POINT('Ctrl Pts',(0.65,-0.575,0.0157371373481999));
#18752=CARTESIAN_POINT('Ctrl Pts',(0.649370620646074,-0.571846918937749,
0.0324967135411165));
#18753=CARTESIAN_POINT('Ctrl Pts',(0.647096224417991,-0.559077918077178,
0.0632828231545124));
#18754=CARTESIAN_POINT('Ctrl Pts',(0.645482573914132,-0.549464140887802,
0.077312554408835));
#18755=CARTESIAN_POINT('Ctrl Pts',(0.642442040715078,-0.527312025401873,
0.099464669894764));
#18756=CARTESIAN_POINT('Ctrl Pts',(0.640815160902589,-0.513282519396725,
0.109078032552995));
#18757=CARTESIAN_POINT('Ctrl Pts',(0.63851034608138,-0.482497190457637,
0.121846732641678));
#18758=CARTESIAN_POINT('Ctrl Pts',(0.637867541108654,-0.465737888992352,
0.125));
#18759=CARTESIAN_POINT('Ctrl Pts',(0.637867541108654,-0.45,0.125));
#18760=CARTESIAN_POINT('',(0.65,-0.325,3.9801020972289E-17));
#18761=CARTESIAN_POINT('Ctrl Pts',(0.65,-0.325,6.93889390390723E-18));
#18762=CARTESIAN_POINT('Ctrl Pts',(0.65,-0.325,-0.0157371373481998));
#18763=CARTESIAN_POINT('Ctrl Pts',(0.649370620646074,-0.328153081062251,
-0.0324967135411164));
#18764=CARTESIAN_POINT('Ctrl Pts',(0.647096224417991,-0.340922081922822,
-0.0632828231545123));
#18765=CARTESIAN_POINT('Ctrl Pts',(0.645482573914132,-0.350535859112198,
-0.0773125544088349));
#18766=CARTESIAN_POINT('Ctrl Pts',(0.642442040715078,-0.372687974598127,
-0.0994646698947639));
#18767=CARTESIAN_POINT('Ctrl Pts',(0.640815160902588,-0.386717480603275,
-0.109078032552995));
#18768=CARTESIAN_POINT('Ctrl Pts',(0.63851034608138,-0.417502809542363,
-0.121846732641678));
#18769=CARTESIAN_POINT('Ctrl Pts',(0.637867541108654,-0.434262111007648,
-0.125));
#18770=CARTESIAN_POINT('Ctrl Pts',(0.637867541108654,-0.465737888992352,
-0.125));
#18771=CARTESIAN_POINT('Ctrl Pts',(0.63851034608138,-0.482497190457637,
-0.121846732641678));
#18772=CARTESIAN_POINT('Ctrl Pts',(0.640815160902589,-0.513282519396725,
-0.109078032552995));
#18773=CARTESIAN_POINT('Ctrl Pts',(0.642442040715078,-0.527312025401873,
-0.0994646698947639));
#18774=CARTESIAN_POINT('Ctrl Pts',(0.645482573914132,-0.549464140887802,
-0.0773125544088348));
#18775=CARTESIAN_POINT('Ctrl Pts',(0.647096224417991,-0.559077918077178,
-0.0632828231545123));
#18776=CARTESIAN_POINT('Ctrl Pts',(0.649370620646074,-0.571846918937749,
-0.0324967135411164));
#18777=CARTESIAN_POINT('Ctrl Pts',(0.65,-0.575,-0.0157371373481998));
#18778=CARTESIAN_POINT('Ctrl Pts',(0.65,-0.575,6.24500451351651E-17));
#18779=CARTESIAN_POINT('Ctrl Pts',(0.637867541108654,-0.45,0.125));
#18780=CARTESIAN_POINT('Ctrl Pts',(0.637867541108654,-0.434262111007648,
0.125));
#18781=CARTESIAN_POINT('Ctrl Pts',(0.63851034608138,-0.417502809542363,
0.121846732641678));
#18782=CARTESIAN_POINT('Ctrl Pts',(0.640815160902589,-0.386717480603274,
0.109078032552995));
#18783=CARTESIAN_POINT('Ctrl Pts',(0.642442040715078,-0.372687974598127,
0.0994646698947639));
#18784=CARTESIAN_POINT('Ctrl Pts',(0.645482573914132,-0.350535859112198,
0.0773125544088348));
#18785=CARTESIAN_POINT('Ctrl Pts',(0.647096224417991,-0.340922081922822,
0.0632828231545123));
#18786=CARTESIAN_POINT('Ctrl Pts',(0.649370620646074,-0.328153081062251,
0.0324967135411164));
#18787=CARTESIAN_POINT('Ctrl Pts',(0.65,-0.325,0.0157371373481998));
#18788=CARTESIAN_POINT('Ctrl Pts',(0.65,-0.325,-6.93889390390723E-18));
#18789=CARTESIAN_POINT('Origin',(0.,-0.1,0.));
#18790=CARTESIAN_POINT('',(-0.65,-0.8,7.9602041944578E-17));
#18791=CARTESIAN_POINT('Origin',(0.,-0.8,0.));
#18792=CARTESIAN_POINT('',(-0.65,-0.1,-7.9602041944578E-17));
#18793=CARTESIAN_POINT('',(-0.65,-0.1,7.9602041944578E-17));
#18794=CARTESIAN_POINT('',(-0.65,-0.1,-7.9602041944578E-17));
#18795=CARTESIAN_POINT('Origin',(0.,-0.1,0.));
#18796=CARTESIAN_POINT('',(0.,-0.575,-0.65));
#18797=CARTESIAN_POINT('',(0.,-0.325,-0.65));
#18798=CARTESIAN_POINT('Ctrl Pts',(-1.73472347597681E-17,-0.575,-0.65));
#18799=CARTESIAN_POINT('Ctrl Pts',(0.0157371373481998,-0.575,-0.65));
#18800=CARTESIAN_POINT('Ctrl Pts',(0.0324967135411164,-0.571846918937749,
-0.649370620646074));
#18801=CARTESIAN_POINT('Ctrl Pts',(0.0632828231545123,-0.559077918077178,
-0.647096224417991));
#18802=CARTESIAN_POINT('Ctrl Pts',(0.0773125544088349,-0.549464140887802,
-0.645482573914132));
#18803=CARTESIAN_POINT('Ctrl Pts',(0.099464669894764,-0.527312025401873,
-0.642442040715078));
#18804=CARTESIAN_POINT('Ctrl Pts',(0.109078032552995,-0.513282519396725,
-0.640815160902589));
#18805=CARTESIAN_POINT('Ctrl Pts',(0.121846732641678,-0.482497190457636,
-0.63851034608138));
#18806=CARTESIAN_POINT('Ctrl Pts',(0.125,-0.465737888992352,-0.637867541108654));
#18807=CARTESIAN_POINT('Ctrl Pts',(0.125,-0.434262111007648,-0.637867541108654));
#18808=CARTESIAN_POINT('Ctrl Pts',(0.121846732641678,-0.417502809542364,
-0.63851034608138));
#18809=CARTESIAN_POINT('Ctrl Pts',(0.109078032552995,-0.386717480603275,
-0.640815160902589));
#18810=CARTESIAN_POINT('Ctrl Pts',(0.099464669894764,-0.372687974598127,
-0.642442040715078));
#18811=CARTESIAN_POINT('Ctrl Pts',(0.0773125544088349,-0.350535859112198,
-0.645482573914132));
#18812=CARTESIAN_POINT('Ctrl Pts',(0.0632828231545123,-0.340922081922822,
-0.647096224417991));
#18813=CARTESIAN_POINT('Ctrl Pts',(0.0324967135411164,-0.328153081062251,
-0.649370620646074));
#18814=CARTESIAN_POINT('Ctrl Pts',(0.0157371373481999,-0.325,-0.65));
#18815=CARTESIAN_POINT('Ctrl Pts',(4.5102810375397E-17,-0.325,-0.65));
#18816=CARTESIAN_POINT('',(-0.125,-0.45,-0.637867541108654));
#18817=CARTESIAN_POINT('Ctrl Pts',(4.85722573273506E-17,-0.325,-0.65));
#18818=CARTESIAN_POINT('Ctrl Pts',(-0.0157371373481997,-0.325,-0.65));
#18819=CARTESIAN_POINT('Ctrl Pts',(-0.0324967135411163,-0.328153081062251,
-0.649370620646074));
#18820=CARTESIAN_POINT('Ctrl Pts',(-0.0632828231545122,-0.340922081922822,
-0.647096224417991));
#18821=CARTESIAN_POINT('Ctrl Pts',(-0.0773125544088348,-0.350535859112198,
-0.645482573914132));
#18822=CARTESIAN_POINT('Ctrl Pts',(-0.0994646698947639,-0.372687974598127,
-0.642442040715078));
#18823=CARTESIAN_POINT('Ctrl Pts',(-0.109078032552995,-0.386717480603274,
-0.640815160902589));
#18824=CARTESIAN_POINT('Ctrl Pts',(-0.121846732641678,-0.417502809542363,
-0.63851034608138));
#18825=CARTESIAN_POINT('Ctrl Pts',(-0.125,-0.434262111007648,-0.637867541108654));
#18826=CARTESIAN_POINT('Ctrl Pts',(-0.125,-0.45,-0.637867541108654));
#18827=CARTESIAN_POINT('Ctrl Pts',(-0.125,-0.45,-0.637867541108654));
#18828=CARTESIAN_POINT('Ctrl Pts',(-0.125,-0.465737888992352,-0.637867541108654));
#18829=CARTESIAN_POINT('Ctrl Pts',(-0.121846732641678,-0.482497190457636,
-0.63851034608138));
#18830=CARTESIAN_POINT('Ctrl Pts',(-0.109078032552995,-0.513282519396725,
-0.640815160902589));
#18831=CARTESIAN_POINT('Ctrl Pts',(-0.099464669894764,-0.527312025401873,
-0.642442040715078));
#18832=CARTESIAN_POINT('Ctrl Pts',(-0.0773125544088349,-0.549464140887802,
-0.645482573914132));
#18833=CARTESIAN_POINT('Ctrl Pts',(-0.0632828231545124,-0.559077918077178,
-0.647096224417991));
#18834=CARTESIAN_POINT('Ctrl Pts',(-0.0324967135411165,-0.571846918937749,
-0.649370620646074));
#18835=CARTESIAN_POINT('Ctrl Pts',(-0.0157371373481998,-0.575,-0.65));
#18836=CARTESIAN_POINT('Ctrl Pts',(-1.73472347597681E-17,-0.575,-0.65));
#18837=CARTESIAN_POINT('',(0.,-0.325,0.65));
#18838=CARTESIAN_POINT('',(0.,-0.575,0.65));
#18839=CARTESIAN_POINT('Ctrl Pts',(2.77555756156289E-17,-0.325,0.65));
#18840=CARTESIAN_POINT('Ctrl Pts',(0.0157371373481998,-0.325,0.65));
#18841=CARTESIAN_POINT('Ctrl Pts',(0.0324967135411164,-0.328153081062251,
0.649370620646074));
#18842=CARTESIAN_POINT('Ctrl Pts',(0.0632828231545123,-0.340922081922822,
0.647096224417991));
#18843=CARTESIAN_POINT('Ctrl Pts',(0.0773125544088349,-0.350535859112198,
0.645482573914132));
#18844=CARTESIAN_POINT('Ctrl Pts',(0.099464669894764,-0.372687974598127,
0.642442040715078));
#18845=CARTESIAN_POINT('Ctrl Pts',(0.109078032552995,-0.386717480603275,
0.640815160902589));
#18846=CARTESIAN_POINT('Ctrl Pts',(0.121846732641678,-0.417502809542364,
0.63851034608138));
#18847=CARTESIAN_POINT('Ctrl Pts',(0.125,-0.434262111007648,0.637867541108654));
#18848=CARTESIAN_POINT('Ctrl Pts',(0.125,-0.465737888992352,0.637867541108654));
#18849=CARTESIAN_POINT('Ctrl Pts',(0.121846732641678,-0.482497190457636,
0.63851034608138));
#18850=CARTESIAN_POINT('Ctrl Pts',(0.109078032552995,-0.513282519396725,
0.640815160902589));
#18851=CARTESIAN_POINT('Ctrl Pts',(0.099464669894764,-0.527312025401873,
0.642442040715078));
#18852=CARTESIAN_POINT('Ctrl Pts',(0.077312554408835,-0.549464140887802,
0.645482573914132));
#18853=CARTESIAN_POINT('Ctrl Pts',(0.0632828231545124,-0.559077918077178,
0.647096224417991));
#18854=CARTESIAN_POINT('Ctrl Pts',(0.0324967135411165,-0.571846918937749,
0.649370620646074));
#18855=CARTESIAN_POINT('Ctrl Pts',(0.0157371373481998,-0.575,0.65));
#18856=CARTESIAN_POINT('Ctrl Pts',(-1.38777878078145E-17,-0.575,0.65));
#18857=CARTESIAN_POINT('',(-0.125,-0.45,0.637867541108654));
#18858=CARTESIAN_POINT('Ctrl Pts',(-1.04083408558608E-17,-0.575,0.65));
#18859=CARTESIAN_POINT('Ctrl Pts',(-0.0157371373481998,-0.575,0.65));
#18860=CARTESIAN_POINT('Ctrl Pts',(-0.0324967135411164,-0.571846918937749,
0.649370620646074));
#18861=CARTESIAN_POINT('Ctrl Pts',(-0.0632828231545123,-0.559077918077178,
0.647096224417991));
#18862=CARTESIAN_POINT('Ctrl Pts',(-0.0773125544088349,-0.549464140887802,
0.645482573914132));
#18863=CARTESIAN_POINT('Ctrl Pts',(-0.099464669894764,-0.527312025401873,
0.642442040715078));
#18864=CARTESIAN_POINT('Ctrl Pts',(-0.109078032552995,-0.513282519396725,
0.640815160902589));
#18865=CARTESIAN_POINT('Ctrl Pts',(-0.121846732641678,-0.482497190457636,
0.63851034608138));
#18866=CARTESIAN_POINT('Ctrl Pts',(-0.125,-0.465737888992352,0.637867541108654));
#18867=CARTESIAN_POINT('Ctrl Pts',(-0.125,-0.45,0.637867541108654));
#18868=CARTESIAN_POINT('Ctrl Pts',(-0.125,-0.45,0.637867541108654));
#18869=CARTESIAN_POINT('Ctrl Pts',(-0.125,-0.434262111007648,0.637867541108654));
#18870=CARTESIAN_POINT('Ctrl Pts',(-0.121846732641678,-0.417502809542363,
0.63851034608138));
#18871=CARTESIAN_POINT('Ctrl Pts',(-0.109078032552995,-0.386717480603274,
0.640815160902589));
#18872=CARTESIAN_POINT('Ctrl Pts',(-0.0994646698947639,-0.372687974598127,
0.642442040715078));
#18873=CARTESIAN_POINT('Ctrl Pts',(-0.0773125544088348,-0.350535859112198,
0.645482573914132));
#18874=CARTESIAN_POINT('Ctrl Pts',(-0.0632828231545122,-0.340922081922822,
0.647096224417991));
#18875=CARTESIAN_POINT('Ctrl Pts',(-0.0324967135411163,-0.328153081062251,
0.649370620646074));
#18876=CARTESIAN_POINT('Ctrl Pts',(-0.0157371373481998,-0.325,0.65));
#18877=CARTESIAN_POINT('Ctrl Pts',(4.5102810375397E-17,-0.325,0.65));
#18878=CARTESIAN_POINT('Origin',(0.,-0.45,0.));
#18879=CARTESIAN_POINT('',(-0.125,-0.45,-0.379967103839267));
#18880=CARTESIAN_POINT('',(-0.125,-0.45,0.));
#18881=CARTESIAN_POINT('',(0.125,-0.45,-0.379967103839267));
#18882=CARTESIAN_POINT('Ctrl Pts',(0.125,-0.45,-0.379967103839267));
#18883=CARTESIAN_POINT('Ctrl Pts',(0.125,-0.465813100629203,-0.379967103839267));
#18884=CARTESIAN_POINT('Ctrl Pts',(0.121817958968287,-0.48260129709332,
-0.381057715344782));
#18885=CARTESIAN_POINT('Ctrl Pts',(0.109029967924066,-0.51336346023721,
-0.384911758361269));
#18886=CARTESIAN_POINT('Ctrl Pts',(0.0994291026068839,-0.527347592689753,
-0.38761064154154));
#18887=CARTESIAN_POINT('Ctrl Pts',(0.0773514949786257,-0.549425200318011,
-0.392612801026882));
#18888=CARTESIAN_POINT('Ctrl Pts',(0.0633657881355918,-0.559029081159106,
-0.395252954914593));
#18889=CARTESIAN_POINT('Ctrl Pts',(0.0325978607437828,-0.571819306519379,
-0.398970551469948));
#18890=CARTESIAN_POINT('Ctrl Pts',(0.0158075115832676,-0.575,-0.4));
#18891=CARTESIAN_POINT('Ctrl Pts',(-0.0158075115832676,-0.575,-0.4));
#18892=CARTESIAN_POINT('Ctrl Pts',(-0.0325978607437828,-0.571819306519379,
-0.398970551469948));
#18893=CARTESIAN_POINT('Ctrl Pts',(-0.0633657881355918,-0.559029081159106,
-0.395252954914593));
#18894=CARTESIAN_POINT('Ctrl Pts',(-0.0773514949786256,-0.549425200318011,
-0.392612801026882));
#18895=CARTESIAN_POINT('Ctrl Pts',(-0.0994291026068839,-0.527347592689753,
-0.38761064154154));
#18896=CARTESIAN_POINT('Ctrl Pts',(-0.109029967924066,-0.51336346023721,
-0.384911758361269));
#18897=CARTESIAN_POINT('Ctrl Pts',(-0.121817958968287,-0.48260129709332,
-0.381057715344782));
#18898=CARTESIAN_POINT('Ctrl Pts',(-0.125,-0.465813100629203,-0.379967103839267));
#18899=CARTESIAN_POINT('Ctrl Pts',(-0.125,-0.45,-0.379967103839267));
#18900=CARTESIAN_POINT('Ctrl Pts',(-0.125,-0.45,-0.379967103839267));
#18901=CARTESIAN_POINT('Ctrl Pts',(-0.125,-0.434186899370797,-0.379967103839267));
#18902=CARTESIAN_POINT('Ctrl Pts',(-0.121817958968287,-0.41739870290668,
-0.381057715344782));
#18903=CARTESIAN_POINT('Ctrl Pts',(-0.109029967924066,-0.38663653976279,
-0.384911758361269));
#18904=CARTESIAN_POINT('Ctrl Pts',(-0.0994291026068839,-0.372652407310247,
-0.38761064154154));
#18905=CARTESIAN_POINT('Ctrl Pts',(-0.0773514949786257,-0.350574799681989,
-0.392612801026882));
#18906=CARTESIAN_POINT('Ctrl Pts',(-0.0633657881355918,-0.340970918840894,
-0.395252954914593));
#18907=CARTESIAN_POINT('Ctrl Pts',(-0.0325978607437829,-0.328180693480621,
-0.398970551469948));
#18908=CARTESIAN_POINT('Ctrl Pts',(-0.0158075115832676,-0.325,-0.4));
#18909=CARTESIAN_POINT('Ctrl Pts',(0.0158075115832675,-0.325,-0.4));
#18910=CARTESIAN_POINT('Ctrl Pts',(0.0325978607437828,-0.328180693480621,
-0.398970551469948));
#18911=CARTESIAN_POINT('Ctrl Pts',(0.0633657881355917,-0.340970918840894,
-0.395252954914593));
#18912=CARTESIAN_POINT('Ctrl Pts',(0.0773514949786256,-0.350574799681989,
-0.392612801026882));
#18913=CARTESIAN_POINT('Ctrl Pts',(0.0994291026068839,-0.372652407310247,
-0.38761064154154));
#18914=CARTESIAN_POINT('Ctrl Pts',(0.109029967924066,-0.38663653976279,
-0.384911758361269));
#18915=CARTESIAN_POINT('Ctrl Pts',(0.121817958968287,-0.41739870290668,
-0.381057715344782));
#18916=CARTESIAN_POINT('Ctrl Pts',(0.125,-0.434186899370797,-0.379967103839267));
#18917=CARTESIAN_POINT('Ctrl Pts',(0.125,-0.45,-0.379967103839267));
#18918=CARTESIAN_POINT('Origin',(0.,-0.45,0.));
#18919=CARTESIAN_POINT('',(0.125,-0.45,0.379967103839267));
#18920=CARTESIAN_POINT('',(-0.125,-0.45,0.379967103839267));
#18921=CARTESIAN_POINT('Ctrl Pts',(0.125,-0.45,0.379967103839267));
#18922=CARTESIAN_POINT('Ctrl Pts',(0.125,-0.434186899370797,0.379967103839267));
#18923=CARTESIAN_POINT('Ctrl Pts',(0.121817958968287,-0.41739870290668,
0.381057715344782));
#18924=CARTESIAN_POINT('Ctrl Pts',(0.109029967924066,-0.38663653976279,
0.384911758361269));
#18925=CARTESIAN_POINT('Ctrl Pts',(0.0994291026068839,-0.372652407310247,
0.38761064154154));
#18926=CARTESIAN_POINT('Ctrl Pts',(0.0773514949786256,-0.350574799681989,
0.392612801026882));
#18927=CARTESIAN_POINT('Ctrl Pts',(0.0633657881355918,-0.340970918840894,
0.395252954914593));
#18928=CARTESIAN_POINT('Ctrl Pts',(0.0325978607437828,-0.328180693480621,
0.398970551469948));
#18929=CARTESIAN_POINT('Ctrl Pts',(0.0158075115832676,-0.325,0.4));
#18930=CARTESIAN_POINT('Ctrl Pts',(-0.0158075115832676,-0.325,0.4));
#18931=CARTESIAN_POINT('Ctrl Pts',(-0.0325978607437828,-0.328180693480621,
0.398970551469948));
#18932=CARTESIAN_POINT('Ctrl Pts',(-0.0633657881355918,-0.340970918840894,
0.395252954914593));
#18933=CARTESIAN_POINT('Ctrl Pts',(-0.0773514949786257,-0.350574799681989,
0.392612801026882));
#18934=CARTESIAN_POINT('Ctrl Pts',(-0.0994291026068839,-0.372652407310247,
0.38761064154154));
#18935=CARTESIAN_POINT('Ctrl Pts',(-0.109029967924066,-0.38663653976279,
0.384911758361269));
#18936=CARTESIAN_POINT('Ctrl Pts',(-0.121817958968287,-0.41739870290668,
0.381057715344782));
#18937=CARTESIAN_POINT('Ctrl Pts',(-0.125,-0.434186899370797,0.379967103839267));
#18938=CARTESIAN_POINT('Ctrl Pts',(-0.125,-0.45,0.379967103839267));
#18939=CARTESIAN_POINT('Ctrl Pts',(-0.125,-0.45,0.379967103839267));
#18940=CARTESIAN_POINT('Ctrl Pts',(-0.125,-0.465813100629203,0.379967103839267));
#18941=CARTESIAN_POINT('Ctrl Pts',(-0.121817958968287,-0.48260129709332,
0.381057715344782));
#18942=CARTESIAN_POINT('Ctrl Pts',(-0.109029967924066,-0.51336346023721,
0.384911758361269));
#18943=CARTESIAN_POINT('Ctrl Pts',(-0.0994291026068839,-0.527347592689753,
0.38761064154154));
#18944=CARTESIAN_POINT('Ctrl Pts',(-0.0773514949786256,-0.549425200318011,
0.392612801026882));
#18945=CARTESIAN_POINT('Ctrl Pts',(-0.0633657881355917,-0.559029081159106,
0.395252954914593));
#18946=CARTESIAN_POINT('Ctrl Pts',(-0.0325978607437828,-0.571819306519379,
0.398970551469948));
#18947=CARTESIAN_POINT('Ctrl Pts',(-0.0158075115832675,-0.575,0.4));
#18948=CARTESIAN_POINT('Ctrl Pts',(0.0158075115832676,-0.575,0.4));
#18949=CARTESIAN_POINT('Ctrl Pts',(0.0325978607437828,-0.571819306519379,
0.398970551469948));
#18950=CARTESIAN_POINT('Ctrl Pts',(0.0633657881355917,-0.559029081159106,
0.395252954914593));
#18951=CARTESIAN_POINT('Ctrl Pts',(0.0773514949786257,-0.549425200318011,
0.392612801026882));
#18952=CARTESIAN_POINT('Ctrl Pts',(0.0994291026068839,-0.527347592689753,
0.38761064154154));
#18953=CARTESIAN_POINT('Ctrl Pts',(0.109029967924066,-0.51336346023721,
0.384911758361269));
#18954=CARTESIAN_POINT('Ctrl Pts',(0.121817958968287,-0.48260129709332,
0.381057715344782));
#18955=CARTESIAN_POINT('Ctrl Pts',(0.125,-0.465813100629203,0.379967103839267));
#18956=CARTESIAN_POINT('Ctrl Pts',(0.125,-0.45,0.379967103839267));
#18957=CARTESIAN_POINT('',(-0.125,-0.45,0.));
#18958=CARTESIAN_POINT('Origin',(0.,0.,0.));
#18959=CARTESIAN_POINT('',(-0.4,-0.8,4.89858719658941E-17));
#18960=CARTESIAN_POINT('Origin',(0.,-0.8,0.));
#18961=CARTESIAN_POINT('',(-0.4,0.,4.89858719658941E-17));
#18962=CARTESIAN_POINT('',(-0.4,0.85,-4.89858719658941E-17));
#18963=CARTESIAN_POINT('',(-0.4,0.,4.89858719658941E-17));
#18964=CARTESIAN_POINT('Origin',(0.,0.85,0.));
#18965=CARTESIAN_POINT('Origin',(0.,-0.8,0.));
#18966=CARTESIAN_POINT('Origin',(0.,0.,0.));
#18967=CARTESIAN_POINT('',(-0.8,0.,9.79717439317883E-17));
#18968=CARTESIAN_POINT('Origin',(0.,0.,0.));
#18969=CARTESIAN_POINT('',(0.595438916863769,0.,0.137993139022126));
#18970=CARTESIAN_POINT('',(0.562830534889751,0.,0.238351419397483));
#18971=CARTESIAN_POINT('Origin',(0.562758945330873,0.,0.182851465569258));
#18972=CARTESIAN_POINT('',(0.523653836874034,0.,0.315240018494132));
#18973=CARTESIAN_POINT('Origin',(0.,0.,0.));
#18974=CARTESIAN_POINT('',(0.461629008549572,0.,0.40060987082025));
#18975=CARTESIAN_POINT('Origin',(0.478711351753049,0.,0.347804155687524));
#18976=CARTESIAN_POINT('',(0.40060987082025,0.,0.461629008549572));
#18977=CARTESIAN_POINT('Origin',(0.,0.,0.));
#18978=CARTESIAN_POINT('',(0.315240018494132,0.,0.523653836874034));
#18979=CARTESIAN_POINT('Origin',(0.347804155687523,0.,0.478711351753049));
#18980=CARTESIAN_POINT('',(0.238351419397483,0.,0.562830534889751));
#18981=CARTESIAN_POINT('Origin',(0.,0.,0.));
#18982=CARTESIAN_POINT('',(0.137993139022126,0.,0.595438916863769));
#18983=CARTESIAN_POINT('Origin',(0.182851465569258,0.,0.562758945330873));
#18984=CARTESIAN_POINT('',(0.0527614703521001,0.,0.608938287003997));
#18985=CARTESIAN_POINT('Origin',(0.,0.,0.));
#18986=CARTESIAN_POINT('',(-0.0527614703521003,0.,0.608938287003997));
#18987=CARTESIAN_POINT('Origin',(-1.08697158783324E-16,0.,0.591719772367581));
#18988=CARTESIAN_POINT('',(-0.137993139022126,0.,0.595438916863769));
#18989=CARTESIAN_POINT('Origin',(0.,0.,0.));
#18990=CARTESIAN_POINT('',(-0.238351419397483,0.,0.562830534889751));
#18991=CARTESIAN_POINT('Origin',(-0.182851465569258,0.,0.562758945330873));
#18992=CARTESIAN_POINT('',(-0.315240018494132,0.,0.523653836874034));
#18993=CARTESIAN_POINT('Origin',(0.,0.,0.));
#18994=CARTESIAN_POINT('',(-0.40060987082025,0.,0.461629008549572));
#18995=CARTESIAN_POINT('Origin',(-0.347804155687524,0.,0.478711351753049));
#18996=CARTESIAN_POINT('',(-0.461629008549572,0.,0.40060987082025));
#18997=CARTESIAN_POINT('Origin',(0.,0.,0.));
#18998=CARTESIAN_POINT('',(-0.523653836874034,0.,0.315240018494132));
#18999=CARTESIAN_POINT('Origin',(-0.478711351753049,0.,0.347804155687524));
#19000=CARTESIAN_POINT('',(-0.562830534889751,0.,0.238351419397483));
#19001=CARTESIAN_POINT('Origin',(0.,0.,0.));
#19002=CARTESIAN_POINT('',(-0.595438916863769,0.,0.137993139022126));
#19003=CARTESIAN_POINT('Origin',(-0.562758945330873,0.,0.182851465569258));
#19004=CARTESIAN_POINT('',(-0.608938287003997,0.,0.0527614703521002));
#19005=CARTESIAN_POINT('Origin',(0.,0.,0.));
#19006=CARTESIAN_POINT('',(-0.608938287003997,0.,-0.0527614703521003));
#19007=CARTESIAN_POINT('Origin',(-0.591719772367581,0.,-7.24647725222159E-17));
#19008=CARTESIAN_POINT('',(-0.595438916863769,0.,-0.137993139022126));
#19009=CARTESIAN_POINT('Origin',(0.,0.,0.));
#19010=CARTESIAN_POINT('',(-0.562830534889751,0.,-0.238351419397483));
#19011=CARTESIAN_POINT('Origin',(-0.562758945330873,0.,-0.182851465569258));
#19012=CARTESIAN_POINT('',(-0.523653836874034,0.,-0.315240018494132));
#19013=CARTESIAN_POINT('Origin',(0.,0.,0.));
#19014=CARTESIAN_POINT('',(-0.461629008549572,0.,-0.40060987082025));
#19015=CARTESIAN_POINT('Origin',(-0.478711351753049,0.,-0.347804155687524));
#19016=CARTESIAN_POINT('',(-0.40060987082025,0.,-0.461629008549572));
#19017=CARTESIAN_POINT('Origin',(0.,0.,0.));
#19018=CARTESIAN_POINT('',(-0.315240018494132,0.,-0.523653836874034));
#19019=CARTESIAN_POINT('Origin',(-0.347804155687524,0.,-0.478711351753049));
#19020=CARTESIAN_POINT('',(-0.238351419397483,0.,-0.562830534889751));
#19021=CARTESIAN_POINT('Origin',(0.,0.,0.));
#19022=CARTESIAN_POINT('',(-0.137993139022126,0.,-0.595438916863769));
#19023=CARTESIAN_POINT('Origin',(-0.182851465569258,0.,-0.562758945330873));
#19024=CARTESIAN_POINT('',(-0.0527614703521002,0.,-0.608938287003997));
#19025=CARTESIAN_POINT('Origin',(0.,0.,0.));
#19026=CARTESIAN_POINT('',(0.0527614703521003,0.,-0.608938287003997));
#19027=CARTESIAN_POINT('Origin',(3.6232386261108E-17,0.,-0.591719772367581));
#19028=CARTESIAN_POINT('',(0.137993139022126,0.,-0.595438916863769));
#19029=CARTESIAN_POINT('Origin',(0.,0.,0.));
#19030=CARTESIAN_POINT('',(0.238351419397483,0.,-0.562830534889751));
#19031=CARTESIAN_POINT('Origin',(0.182851465569258,0.,-0.562758945330873));
#19032=CARTESIAN_POINT('',(0.315240018494132,0.,-0.523653836874034));
#19033=CARTESIAN_POINT('Origin',(0.,0.,0.));
#19034=CARTESIAN_POINT('',(0.40060987082025,0.,-0.461629008549572));
#19035=CARTESIAN_POINT('Origin',(0.347804155687524,0.,-0.478711351753049));
#19036=CARTESIAN_POINT('',(0.461629008549572,0.,-0.40060987082025));
#19037=CARTESIAN_POINT('Origin',(0.,0.,0.));
#19038=CARTESIAN_POINT('',(0.523653836874034,0.,-0.315240018494132));
#19039=CARTESIAN_POINT('Origin',(0.478711351753049,0.,-0.347804155687524));
#19040=CARTESIAN_POINT('',(0.562830534889751,0.,-0.238351419397483));
#19041=CARTESIAN_POINT('Origin',(0.,0.,0.));
#19042=CARTESIAN_POINT('',(0.595438916863769,0.,-0.137993139022126));
#19043=CARTESIAN_POINT('Origin',(0.562758945330873,0.,-0.182851465569258));
#19044=CARTESIAN_POINT('',(0.608938287003997,0.,-0.0527614703521001));
#19045=CARTESIAN_POINT('Origin',(0.,0.,0.));
#19046=CARTESIAN_POINT('',(0.608938287003997,0.,0.0527614703521001));
#19047=CARTESIAN_POINT('Origin',(0.591719772367581,0.,0.));
#19048=CARTESIAN_POINT('Origin',(0.,0.,0.));
#19049=CARTESIAN_POINT('Origin',(0.,0.,0.));
#19050=CARTESIAN_POINT('',(-0.8,-0.1,9.79717439317883E-17));
#19051=CARTESIAN_POINT('Origin',(0.,-0.1,0.));
#19052=CARTESIAN_POINT('',(-0.8,0.,-9.79717439317883E-17));
#19053=CARTESIAN_POINT('Origin',(0.,-0.1,0.));
#19054=CARTESIAN_POINT('Origin',(0.,0.75,0.));
#19055=CARTESIAN_POINT('',(-0.8,0.75,9.79717439317883E-17));
#19056=CARTESIAN_POINT('Origin',(0.,0.75,0.));
#19057=CARTESIAN_POINT('',(0.562830534889751,0.75,0.238351419397483));
#19058=CARTESIAN_POINT('',(0.595438916863769,0.75,0.137993139022126));
#19059=CARTESIAN_POINT('Origin',(0.562758945330873,0.75,0.182851465569258));
#19060=CARTESIAN_POINT('',(0.608938287003997,0.75,0.0527614703521002));
#19061=CARTESIAN_POINT('Origin',(0.,0.75,0.));
#19062=CARTESIAN_POINT('',(0.608938287003997,0.75,-0.0527614703521002));
#19063=CARTESIAN_POINT('Origin',(0.591719772367581,0.75,0.));
#19064=CARTESIAN_POINT('',(0.595438916863769,0.75,-0.137993139022126));
#19065=CARTESIAN_POINT('Origin',(0.,0.75,0.));
#19066=CARTESIAN_POINT('',(0.562830534889751,0.75,-0.238351419397483));
#19067=CARTESIAN_POINT('Origin',(0.562758945330873,0.75,-0.182851465569258));
#19068=CARTESIAN_POINT('',(0.523653836874034,0.75,-0.315240018494132));
#19069=CARTESIAN_POINT('Origin',(0.,0.75,0.));
#19070=CARTESIAN_POINT('',(0.461629008549572,0.75,-0.40060987082025));
#19071=CARTESIAN_POINT('Origin',(0.478711351753049,0.75,-0.347804155687524));
#19072=CARTESIAN_POINT('',(0.40060987082025,0.75,-0.461629008549572));
#19073=CARTESIAN_POINT('Origin',(0.,0.75,0.));
#19074=CARTESIAN_POINT('',(0.315240018494132,0.75,-0.523653836874034));
#19075=CARTESIAN_POINT('Origin',(0.347804155687524,0.75,-0.478711351753049));
#19076=CARTESIAN_POINT('',(0.238351419397483,0.75,-0.562830534889751));
#19077=CARTESIAN_POINT('Origin',(0.,0.75,0.));
#19078=CARTESIAN_POINT('',(0.137993139022126,0.75,-0.595438916863769));
#19079=CARTESIAN_POINT('Origin',(0.182851465569258,0.75,-0.562758945330873));
#19080=CARTESIAN_POINT('',(0.0527614703521003,0.75,-0.608938287003997));
#19081=CARTESIAN_POINT('Origin',(0.,0.75,0.));
#19082=CARTESIAN_POINT('',(-0.0527614703521002,0.75,-0.608938287003997));
#19083=CARTESIAN_POINT('Origin',(3.6232386261108E-17,0.75,-0.591719772367581));
#19084=CARTESIAN_POINT('',(-0.137993139022126,0.75,-0.595438916863769));
#19085=CARTESIAN_POINT('Origin',(0.,0.75,0.));
#19086=CARTESIAN_POINT('',(-0.238351419397483,0.75,-0.562830534889751));
#19087=CARTESIAN_POINT('Origin',(-0.182851465569258,0.75,-0.562758945330873));
#19088=CARTESIAN_POINT('',(-0.315240018494132,0.75,-0.523653836874034));
#19089=CARTESIAN_POINT('Origin',(0.,0.75,0.));
#19090=CARTESIAN_POINT('',(-0.40060987082025,0.75,-0.461629008549572));
#19091=CARTESIAN_POINT('Origin',(-0.347804155687524,0.75,-0.478711351753049));
#19092=CARTESIAN_POINT('',(-0.461629008549572,0.75,-0.40060987082025));
#19093=CARTESIAN_POINT('Origin',(0.,0.75,0.));
#19094=CARTESIAN_POINT('',(-0.523653836874034,0.75,-0.315240018494132));
#19095=CARTESIAN_POINT('Origin',(-0.478711351753049,0.75,-0.347804155687524));
#19096=CARTESIAN_POINT('',(-0.562830534889751,0.75,-0.238351419397483));
#19097=CARTESIAN_POINT('Origin',(0.,0.75,0.));
#19098=CARTESIAN_POINT('',(-0.595438916863769,0.75,-0.137993139022126));
#19099=CARTESIAN_POINT('Origin',(-0.562758945330873,0.75,-0.182851465569258));
#19100=CARTESIAN_POINT('',(-0.608938287003997,0.75,-0.0527614703521003));
#19101=CARTESIAN_POINT('Origin',(0.,0.75,0.));
#19102=CARTESIAN_POINT('',(-0.608938287003997,0.75,0.0527614703521002));
#19103=CARTESIAN_POINT('Origin',(-0.591719772367581,0.75,-7.24647725222159E-17));
#19104=CARTESIAN_POINT('',(-0.595438916863769,0.75,0.137993139022126));
#19105=CARTESIAN_POINT('Origin',(0.,0.75,0.));
#19106=CARTESIAN_POINT('',(-0.562830534889751,0.75,0.238351419397483));
#19107=CARTESIAN_POINT('Origin',(-0.562758945330873,0.75,0.182851465569258));
#19108=CARTESIAN_POINT('',(-0.523653836874034,0.75,0.315240018494132));
#19109=CARTESIAN_POINT('Origin',(0.,0.75,0.));
#19110=CARTESIAN_POINT('',(-0.461629008549572,0.75,0.40060987082025));
#19111=CARTESIAN_POINT('Origin',(-0.478711351753049,0.75,0.347804155687524));
#19112=CARTESIAN_POINT('',(-0.40060987082025,0.75,0.461629008549572));
#19113=CARTESIAN_POINT('Origin',(0.,0.75,0.));
#19114=CARTESIAN_POINT('',(-0.315240018494132,0.75,0.523653836874034));
#19115=CARTESIAN_POINT('Origin',(-0.347804155687524,0.75,0.478711351753049));
#19116=CARTESIAN_POINT('',(-0.238351419397483,0.75,0.562830534889751));
#19117=CARTESIAN_POINT('Origin',(0.,0.75,0.));
#19118=CARTESIAN_POINT('',(-0.137993139022126,0.75,0.595438916863769));
#19119=CARTESIAN_POINT('Origin',(-0.182851465569258,0.75,0.562758945330873));
#19120=CARTESIAN_POINT('',(-0.0527614703521003,0.75,0.608938287003997));
#19121=CARTESIAN_POINT('Origin',(0.,0.75,0.));
#19122=CARTESIAN_POINT('',(0.0527614703521001,0.75,0.608938287003997));
#19123=CARTESIAN_POINT('Origin',(-1.08697158783324E-16,0.75,0.591719772367581));
#19124=CARTESIAN_POINT('',(0.137993139022126,0.75,0.595438916863769));
#19125=CARTESIAN_POINT('Origin',(0.,0.75,0.));
#19126=CARTESIAN_POINT('',(0.238351419397483,0.75,0.562830534889751));
#19127=CARTESIAN_POINT('Origin',(0.182851465569258,0.75,0.562758945330873));
#19128=CARTESIAN_POINT('',(0.315240018494132,0.75,0.523653836874034));
#19129=CARTESIAN_POINT('Origin',(0.,0.75,0.));
#19130=CARTESIAN_POINT('',(0.40060987082025,0.75,0.461629008549572));
#19131=CARTESIAN_POINT('Origin',(0.347804155687523,0.75,0.478711351753049));
#19132=CARTESIAN_POINT('',(0.461629008549572,0.75,0.40060987082025));
#19133=CARTESIAN_POINT('Origin',(0.,0.75,0.));
#19134=CARTESIAN_POINT('',(0.523653836874034,0.75,0.315240018494132));
#19135=CARTESIAN_POINT('Origin',(0.478711351753049,0.75,0.347804155687524));
#19136=CARTESIAN_POINT('Origin',(0.,0.75,0.));
#19137=CARTESIAN_POINT('Origin',(0.,0.75,0.));
#19138=CARTESIAN_POINT('',(-0.8,0.85,9.79717439317883E-17));
#19139=CARTESIAN_POINT('Origin',(0.,0.85,0.));
#19140=CARTESIAN_POINT('',(-0.8,0.75,9.79717439317883E-17));
#19141=CARTESIAN_POINT('Origin',(0.,0.85,0.));
#19142=CARTESIAN_POINT('Origin',(0.562758945330873,0.,0.182851465569258));
#19143=CARTESIAN_POINT('',(0.595438916863769,0.,0.137993139022126));
#19144=CARTESIAN_POINT('',(0.562830534889751,0.,0.238351419397483));
#19145=CARTESIAN_POINT('Origin',(0.,0.,0.));
#19146=CARTESIAN_POINT('',(0.523653836874034,0.,0.315240018494132));
#19147=CARTESIAN_POINT('Origin',(0.478711351753049,0.,0.347804155687524));
#19148=CARTESIAN_POINT('',(0.461629008549572,0.,0.40060987082025));
#19149=CARTESIAN_POINT('Origin',(0.,0.,0.));
#19150=CARTESIAN_POINT('',(0.40060987082025,0.,0.461629008549572));
#19151=CARTESIAN_POINT('Origin',(0.347804155687523,0.,0.478711351753049));
#19152=CARTESIAN_POINT('',(0.315240018494132,0.,0.523653836874034));
#19153=CARTESIAN_POINT('Origin',(0.,0.,0.));
#19154=CARTESIAN_POINT('',(0.238351419397483,0.,0.562830534889751));
#19155=CARTESIAN_POINT('Origin',(0.182851465569258,0.,0.562758945330873));
#19156=CARTESIAN_POINT('',(0.137993139022126,0.,0.595438916863769));
#19157=CARTESIAN_POINT('Origin',(0.,0.,0.));
#19158=CARTESIAN_POINT('',(0.0527614703521,0.,0.608938287003997));
#19159=CARTESIAN_POINT('Origin',(-1.08697158783324E-16,0.,0.591719772367581));
#19160=CARTESIAN_POINT('',(-0.0527614703521002,0.,0.608938287003997));
#19161=CARTESIAN_POINT('Origin',(0.,0.,0.));
#19162=CARTESIAN_POINT('',(-0.137993139022126,0.,0.595438916863769));
#19163=CARTESIAN_POINT('Origin',(-0.182851465569258,0.,0.562758945330873));
#19164=CARTESIAN_POINT('',(-0.238351419397483,0.,0.562830534889751));
#19165=CARTESIAN_POINT('Origin',(0.,0.,0.));
#19166=CARTESIAN_POINT('',(-0.315240018494132,0.,0.523653836874034));
#19167=CARTESIAN_POINT('Origin',(-0.347804155687524,0.,0.478711351753049));
#19168=CARTESIAN_POINT('',(-0.40060987082025,0.,0.461629008549572));
#19169=CARTESIAN_POINT('Origin',(0.,0.,0.));
#19170=CARTESIAN_POINT('',(-0.461629008549572,0.,0.40060987082025));
#19171=CARTESIAN_POINT('Origin',(-0.478711351753049,0.,0.347804155687524));
#19172=CARTESIAN_POINT('',(-0.523653836874034,0.,0.315240018494132));
#19173=CARTESIAN_POINT('Origin',(0.,0.,0.));
#19174=CARTESIAN_POINT('',(-0.562830534889751,0.,0.238351419397483));
#19175=CARTESIAN_POINT('Origin',(-0.562758945330873,0.,0.182851465569258));
#19176=CARTESIAN_POINT('',(-0.595438916863769,0.,0.137993139022126));
#19177=CARTESIAN_POINT('Origin',(0.,0.,0.));
#19178=CARTESIAN_POINT('',(-0.608938287003997,0.,0.0527614703521));
#19179=CARTESIAN_POINT('Origin',(-0.591719772367581,0.,-7.24647725222159E-17));
#19180=CARTESIAN_POINT('',(-0.608938287003997,0.,-0.0527614703521002));
#19181=CARTESIAN_POINT('Origin',(0.,0.,0.));
#19182=CARTESIAN_POINT('',(-0.595438916863769,0.,-0.137993139022126));
#19183=CARTESIAN_POINT('Origin',(-0.562758945330873,0.,-0.182851465569258));
#19184=CARTESIAN_POINT('',(-0.562830534889751,0.,-0.238351419397483));
#19185=CARTESIAN_POINT('Origin',(0.,0.,0.));
#19186=CARTESIAN_POINT('',(-0.523653836874034,0.,-0.315240018494132));
#19187=CARTESIAN_POINT('Origin',(-0.478711351753049,0.,-0.347804155687524));
#19188=CARTESIAN_POINT('',(-0.461629008549572,0.,-0.40060987082025));
#19189=CARTESIAN_POINT('Origin',(0.,0.,0.));
#19190=CARTESIAN_POINT('',(-0.40060987082025,0.,-0.461629008549572));
#19191=CARTESIAN_POINT('Origin',(-0.347804155687524,0.,-0.478711351753049));
#19192=CARTESIAN_POINT('',(-0.315240018494132,0.,-0.523653836874034));
#19193=CARTESIAN_POINT('Origin',(0.,0.,0.));
#19194=CARTESIAN_POINT('',(-0.238351419397483,0.,-0.562830534889751));
#19195=CARTESIAN_POINT('Origin',(-0.182851465569258,0.,-0.562758945330873));
#19196=CARTESIAN_POINT('',(-0.137993139022126,0.,-0.595438916863769));
#19197=CARTESIAN_POINT('Origin',(0.,0.,0.));
#19198=CARTESIAN_POINT('',(-0.0527614703521,0.,-0.608938287003997));
#19199=CARTESIAN_POINT('Origin',(3.6232386261108E-17,0.,-0.591719772367581));
#19200=CARTESIAN_POINT('',(0.0527614703521001,0.,-0.608938287003997));
#19201=CARTESIAN_POINT('Origin',(0.,0.,0.));
#19202=CARTESIAN_POINT('',(0.137993139022126,0.,-0.595438916863769));
#19203=CARTESIAN_POINT('Origin',(0.182851465569258,0.,-0.562758945330873));
#19204=CARTESIAN_POINT('',(0.238351419397483,0.,-0.562830534889751));
#19205=CARTESIAN_POINT('Origin',(0.,0.,0.));
#19206=CARTESIAN_POINT('',(0.315240018494132,0.,-0.523653836874034));
#19207=CARTESIAN_POINT('Origin',(0.347804155687524,0.,-0.478711351753049));
#19208=CARTESIAN_POINT('',(0.40060987082025,0.,-0.461629008549572));
#19209=CARTESIAN_POINT('Origin',(0.,0.,0.));
#19210=CARTESIAN_POINT('',(0.461629008549572,0.,-0.40060987082025));
#19211=CARTESIAN_POINT('Origin',(0.478711351753049,0.,-0.347804155687524));
#19212=CARTESIAN_POINT('',(0.523653836874034,0.,-0.315240018494132));
#19213=CARTESIAN_POINT('Origin',(0.,0.,0.));
#19214=CARTESIAN_POINT('',(0.562830534889751,0.,-0.238351419397483));
#19215=CARTESIAN_POINT('Origin',(0.562758945330873,0.,-0.182851465569258));
#19216=CARTESIAN_POINT('',(0.595438916863769,0.,-0.137993139022126));
#19217=CARTESIAN_POINT('Origin',(0.,0.,0.));
#19218=CARTESIAN_POINT('',(0.608938287003997,0.,0.0527614703521001));
#19219=CARTESIAN_POINT('Origin',(0.591719772367581,0.,0.));
#19220=CARTESIAN_POINT('',(0.608938287003997,0.,-0.0527614703521001));
#19221=CARTESIAN_POINT('Origin',(0.,0.,0.));
#19222=CARTESIAN_POINT('',(0.,0.,0.));
#19223=CARTESIAN_POINT('',(0.,0.,0.));
#19224=CARTESIAN_POINT('Origin',(15.5,-1.8,2.3));
#19225=CARTESIAN_POINT('',(15.1,-1.8,2.4));
#19226=CARTESIAN_POINT('Origin',(15.5,-1.8,2.4));
#19227=CARTESIAN_POINT('',(15.1,-1.8,2.8));
#19228=CARTESIAN_POINT('',(15.1,-1.8,2.3));
#19229=CARTESIAN_POINT('Origin',(15.5,-1.8,2.8));
#19230=CARTESIAN_POINT('Origin',(15.5,-1.8,2.8));
#19231=CARTESIAN_POINT('',(15.275,-1.8,2.8));
#19232=CARTESIAN_POINT('Origin',(15.5,-1.8,2.8));
#19233=CARTESIAN_POINT('Origin',(16.5,-1.8,2.3));
#19234=CARTESIAN_POINT('',(16.1,-1.8,2.4));
#19235=CARTESIAN_POINT('Origin',(16.5,-1.8,2.4));
#19236=CARTESIAN_POINT('',(16.1,-1.8,2.8));
#19237=CARTESIAN_POINT('',(16.1,-1.8,2.3));
#19238=CARTESIAN_POINT('Origin',(16.5,-1.8,2.8));
#19239=CARTESIAN_POINT('Origin',(16.5,-1.8,2.8));
#19240=CARTESIAN_POINT('',(16.275,-1.8,2.8));
#19241=CARTESIAN_POINT('Origin',(16.5,-1.8,2.8));
#19242=CARTESIAN_POINT('Origin',(15.5,-1.8,2.3));
#19243=CARTESIAN_POINT('',(15.275,-1.8,3.6));
#19244=CARTESIAN_POINT('',(15.275,-1.8,2.3));
#19245=CARTESIAN_POINT('Origin',(15.5,-1.8,3.6));
#19246=CARTESIAN_POINT('Origin',(16.5,-1.8,2.3));
#19247=CARTESIAN_POINT('',(16.275,-1.8,3.6));
#19248=CARTESIAN_POINT('',(16.275,-1.8,2.3));
#19249=CARTESIAN_POINT('Origin',(16.5,-1.8,3.6));
#19250=CARTESIAN_POINT('Origin',(17.5,-1.9,2.3));
#19251=CARTESIAN_POINT('',(17.225,-1.9,2.4));
#19252=CARTESIAN_POINT('Origin',(17.5,-1.9,2.4));
#19253=CARTESIAN_POINT('',(17.225,-1.9,3.6));
#19254=CARTESIAN_POINT('',(17.225,-1.9,2.3));
#19255=CARTESIAN_POINT('Origin',(17.5,-1.9,3.6));
#19256=CARTESIAN_POINT('Origin',(14.5,1.9,2.3));
#19257=CARTESIAN_POINT('',(14.225,1.9,2.4));
#19258=CARTESIAN_POINT('Origin',(14.5,1.9,2.4));
#19259=CARTESIAN_POINT('',(14.225,1.9,3.6));
#19260=CARTESIAN_POINT('',(14.225,1.9,2.3));
#19261=CARTESIAN_POINT('Origin',(14.5,1.9,3.6));
#19262=CARTESIAN_POINT('Origin',(14.5,-1.9,2.3));
#19263=CARTESIAN_POINT('',(14.225,-1.9,2.4));
#19264=CARTESIAN_POINT('Origin',(14.5,-1.9,2.4));
#19265=CARTESIAN_POINT('',(14.225,-1.9,3.6));
#19266=CARTESIAN_POINT('',(14.225,-1.9,2.3));
#19267=CARTESIAN_POINT('Origin',(14.5,-1.9,3.6));
#19268=CARTESIAN_POINT('Origin',(17.5,1.9,2.3));
#19269=CARTESIAN_POINT('',(17.225,1.9,2.4));
#19270=CARTESIAN_POINT('Origin',(17.5,1.9,2.4));
#19271=CARTESIAN_POINT('',(17.225,1.9,3.6));
#19272=CARTESIAN_POINT('',(17.225,1.9,2.3));
#19273=CARTESIAN_POINT('Origin',(17.5,1.9,3.6));
#19274=CARTESIAN_POINT('Origin',(19.5,3.2,2.4));
#19275=CARTESIAN_POINT('',(19.5,3.2,2.4));
#19276=CARTESIAN_POINT('',(12.5,3.2,2.4));
#19277=CARTESIAN_POINT('',(19.5,3.2,2.4));
#19278=CARTESIAN_POINT('',(12.5,3.2,3.6));
#19279=CARTESIAN_POINT('',(12.5,3.2,2.4));
#19280=CARTESIAN_POINT('',(19.5,3.2,3.6));
#19281=CARTESIAN_POINT('',(19.5,3.2,3.6));
#19282=CARTESIAN_POINT('',(19.5,3.2,2.4));
#19283=CARTESIAN_POINT('Origin',(19.5,-3.2,2.4));
#19284=CARTESIAN_POINT('',(19.5,-3.2,2.4));
#19285=CARTESIAN_POINT('',(19.5,-3.2,2.4));
#19286=CARTESIAN_POINT('',(19.5,-3.2,3.6));
#19287=CARTESIAN_POINT('',(19.5,-3.2,3.6));
#19288=CARTESIAN_POINT('',(19.5,-3.2,2.4));
#19289=CARTESIAN_POINT('Origin',(12.5,-3.2,2.4));
#19290=CARTESIAN_POINT('',(12.5,-3.2,2.4));
#19291=CARTESIAN_POINT('',(12.5,-3.2,2.4));
#19292=CARTESIAN_POINT('',(12.5,-3.2,3.6));
#19293=CARTESIAN_POINT('',(12.5,-3.2,3.6));
#19294=CARTESIAN_POINT('',(12.5,-3.2,2.4));
#19295=CARTESIAN_POINT('Origin',(12.5,3.2,2.4));
#19296=CARTESIAN_POINT('',(12.5,3.2,2.4));
#19297=CARTESIAN_POINT('',(12.5,3.2,3.6));
#19298=CARTESIAN_POINT('Origin',(16.,0.,3.6));
#19299=CARTESIAN_POINT('Origin',(16.,0.,2.4));
#19300=CARTESIAN_POINT('',(0.,0.,0.));
#19301=CARTESIAN_POINT('Origin',(15.5,-1.8,3.5));
#19302=CARTESIAN_POINT('',(15.335,-1.8,3.6));
#19303=CARTESIAN_POINT('Origin',(15.5,-1.8,3.6));
#19304=CARTESIAN_POINT('',(15.335,-1.8,4.5));
#19305=CARTESIAN_POINT('',(15.335,-1.8,3.5));
#19306=CARTESIAN_POINT('Origin',(15.5,-1.8,4.5));
#19307=CARTESIAN_POINT('Origin',(15.5,-1.8,4.5));
#19308=CARTESIAN_POINT('Origin',(16.5,-1.8,3.5));
#19309=CARTESIAN_POINT('',(16.335,-1.8,3.6));
#19310=CARTESIAN_POINT('Origin',(16.5,-1.8,3.6));
#19311=CARTESIAN_POINT('',(16.335,-1.8,4.5));
#19312=CARTESIAN_POINT('',(16.335,-1.8,3.5));
#19313=CARTESIAN_POINT('Origin',(16.5,-1.8,4.5));
#19314=CARTESIAN_POINT('Origin',(16.5,-1.8,4.5));
#19315=CARTESIAN_POINT('Origin',(14.5,-1.9,4.5));
#19316=CARTESIAN_POINT('',(14.8316624790355,-1.4,4.5));
#19317=CARTESIAN_POINT('',(14.5,-1.4,4.5));
#19318=CARTESIAN_POINT('',(16.,-1.4,4.5));
#19319=CARTESIAN_POINT('',(15.0196152422707,-2.2,4.5));
#19320=CARTESIAN_POINT('Origin',(14.5,-1.9,4.5));
#19321=CARTESIAN_POINT('',(14.5,-2.2,4.5));
#19322=CARTESIAN_POINT('',(14.5,-2.2,4.5));
#19323=CARTESIAN_POINT('',(14.5,-1.65,4.5));
#19324=CARTESIAN_POINT('Origin',(14.5,-1.9,3.5));
#19325=CARTESIAN_POINT('',(14.8316624790355,-1.4,3.6));
#19326=CARTESIAN_POINT('',(14.8316624790355,-1.4,3.5));
#19327=CARTESIAN_POINT('',(15.0196152422707,-2.2,3.6));
#19328=CARTESIAN_POINT('Origin',(14.5,-1.9,3.6));
#19329=CARTESIAN_POINT('',(15.0196152422707,-2.2,3.5));
#19330=CARTESIAN_POINT('Origin',(17.5,-1.9,3.5));
#19331=CARTESIAN_POINT('',(17.1683375209645,-1.4,4.5));
#19332=CARTESIAN_POINT('',(17.1683375209645,-1.4,3.6));
#19333=CARTESIAN_POINT('',(17.1683375209645,-1.4,3.5));
#19334=CARTESIAN_POINT('',(16.9803847577293,-2.2,4.5));
#19335=CARTESIAN_POINT('Origin',(17.5,-1.9,4.5));
#19336=CARTESIAN_POINT('',(16.9803847577293,-2.2,3.6));
#19337=CARTESIAN_POINT('',(16.9803847577293,-2.2,3.5));
#19338=CARTESIAN_POINT('Origin',(17.5,-1.9,3.6));
#19339=CARTESIAN_POINT('Origin',(17.5,-1.9,4.5));
#19340=CARTESIAN_POINT('',(17.5,-1.4,4.5));
#19341=CARTESIAN_POINT('',(17.5,-1.4,4.5));
#19342=CARTESIAN_POINT('',(17.5,-2.2,4.5));
#19343=CARTESIAN_POINT('',(17.5,-2.05,4.5));
#19344=CARTESIAN_POINT('',(16.,-2.2,4.5));
#19345=CARTESIAN_POINT('Origin',(14.5,-1.4,3.6));
#19346=CARTESIAN_POINT('',(14.5,-2.2,7.73661977));
#19347=CARTESIAN_POINT('',(14.5,-2.2,3.6));
#19348=CARTESIAN_POINT('',(14.5,-3.425,7.73661977));
#19349=CARTESIAN_POINT('',(14.5,-1.4,7.73661977));
#19350=CARTESIAN_POINT('',(14.5,-3.425,8.13661977));
#19351=CARTESIAN_POINT('',(14.5,-3.425,7.73661977));
#19352=CARTESIAN_POINT('',(14.5,-1.4,8.13661977));
#19353=CARTESIAN_POINT('',(14.5,-1.4,8.13661977));
#19354=CARTESIAN_POINT('',(14.5,-1.4,3.6));
#19355=CARTESIAN_POINT('Origin',(14.5,-2.2,3.6));
#19356=CARTESIAN_POINT('',(14.5,-2.2,3.6));
#19357=CARTESIAN_POINT('',(17.5,-2.2,7.73661977));
#19358=CARTESIAN_POINT('',(17.5,-2.2,3.6));
#19359=CARTESIAN_POINT('',(15.25,-2.2,7.73661977));
#19360=CARTESIAN_POINT('Origin',(15.5,-1.8,6.8));
#19361=CARTESIAN_POINT('',(15.335,-1.8,6.8));
#19362=CARTESIAN_POINT('Origin',(15.5,-1.8,6.8));
#19363=CARTESIAN_POINT('',(15.335,-1.8,8.13661977));
#19364=CARTESIAN_POINT('',(15.335,-1.8,6.8));
#19365=CARTESIAN_POINT('Origin',(15.5,-1.8,8.13661977));
#19366=CARTESIAN_POINT('Origin',(15.5,-1.8,6.8));
#19367=CARTESIAN_POINT('Origin',(16.5,-1.8,6.8));
#19368=CARTESIAN_POINT('',(16.335,-1.8,6.8));
#19369=CARTESIAN_POINT('Origin',(16.5,-1.8,6.8));
#19370=CARTESIAN_POINT('',(16.335,-1.8,8.13661977));
#19371=CARTESIAN_POINT('',(16.335,-1.8,6.8));
#19372=CARTESIAN_POINT('Origin',(16.5,-1.8,8.13661977));
#19373=CARTESIAN_POINT('Origin',(16.5,-1.8,6.8));
#19374=CARTESIAN_POINT('Origin',(16.,-2.4125,8.13661977));
#19375=CARTESIAN_POINT('',(17.5,-3.425,8.13661977));
#19376=CARTESIAN_POINT('',(14.5,-3.425,8.13661977));
#19377=CARTESIAN_POINT('',(17.5,-1.4,8.13661977));
#19378=CARTESIAN_POINT('',(17.5,-3.425,8.13661977));
#19379=CARTESIAN_POINT('',(17.5,-1.4,8.13661977));
#19380=CARTESIAN_POINT('Origin',(14.5,-3.425,7.73661977));
#19381=CARTESIAN_POINT('',(17.5,-3.425,7.73661977));
#19382=CARTESIAN_POINT('',(14.5,-3.425,7.73661977));
#19383=CARTESIAN_POINT('',(17.5,-3.425,7.73661977));
#19384=CARTESIAN_POINT('Origin',(16.,-2.4125,7.73661977));
#19385=CARTESIAN_POINT('',(17.5,-3.425,7.73661977));
#19386=CARTESIAN_POINT('Origin',(17.5,-1.4,3.6));
#19387=CARTESIAN_POINT('',(17.5,-1.4,3.6));
#19388=CARTESIAN_POINT('',(17.5,-1.4,3.6));
#19389=CARTESIAN_POINT('Origin',(17.5,-2.2,3.6));
#19390=CARTESIAN_POINT('Origin',(16.,-1.8,3.6));
#19391=CARTESIAN_POINT('',(0.,0.,0.));
#19392=CARTESIAN_POINT('Origin',(17.5,-2.2,7.23661977));
#19393=CARTESIAN_POINT('',(17.5,-2.2,7.23661977));
#19394=CARTESIAN_POINT('',(14.5,-2.2,7.23661977));
#19395=CARTESIAN_POINT('',(17.5,-2.2,7.23661977));
#19396=CARTESIAN_POINT('',(14.5,-2.2,7.63661977));
#19397=CARTESIAN_POINT('',(14.5,-2.2,7.23661977));
#19398=CARTESIAN_POINT('',(17.5,-2.2,7.63661977));
#19399=CARTESIAN_POINT('',(17.5,-2.2,7.63661977));
#19400=CARTESIAN_POINT('',(17.5,-2.2,7.23661977));
#19401=CARTESIAN_POINT('Origin',(17.5,-3.425,7.23661977));
#19402=CARTESIAN_POINT('',(17.5,-3.425,7.23661977));
#19403=CARTESIAN_POINT('',(17.5,-3.425,7.23661977));
#19404=CARTESIAN_POINT('',(17.5,-3.425,7.63661977));
#19405=CARTESIAN_POINT('',(17.5,-3.425,7.63661977));
#19406=CARTESIAN_POINT('',(17.5,-3.425,7.23661977));
#19407=CARTESIAN_POINT('Origin',(14.5,-3.425,7.23661977));
#19408=CARTESIAN_POINT('',(14.5,-3.425,7.23661977));
#19409=CARTESIAN_POINT('',(14.5,-3.425,7.23661977));
#19410=CARTESIAN_POINT('',(14.5,-3.425,7.63661977));
#19411=CARTESIAN_POINT('',(14.5,-3.425,7.63661977));
#19412=CARTESIAN_POINT('',(14.5,-3.425,7.23661977));
#19413=CARTESIAN_POINT('Origin',(14.5,-2.2,7.23661977));
#19414=CARTESIAN_POINT('',(14.5,-2.2,7.23661977));
#19415=CARTESIAN_POINT('',(14.5,-2.2,7.63661977));
#19416=CARTESIAN_POINT('Origin',(16.,-2.8125,7.63661977));
#19417=CARTESIAN_POINT('Origin',(16.,-2.8125,7.23661977));
#19418=CARTESIAN_POINT('',(0.,0.,0.));
#19419=CARTESIAN_POINT('',(0.,0.,0.));
#19420=CARTESIAN_POINT('Origin',(1.5,-1.9,1.7));
#19421=CARTESIAN_POINT('',(1.56403124237433,-1.7,1.7));
#19422=CARTESIAN_POINT('',(1.43596875762567,-1.7,1.7));
#19423=CARTESIAN_POINT('',(0.75,-1.7,1.7));
#19424=CARTESIAN_POINT('Origin',(1.5,-1.9,1.7));
#19425=CARTESIAN_POINT('Origin',(1.5,-1.9,1.7));
#19426=CARTESIAN_POINT('',(1.56403124237433,-1.7,1.75));
#19427=CARTESIAN_POINT('',(1.56403124237433,-1.7,1.7));
#19428=CARTESIAN_POINT('',(1.29,-1.9,1.75));
#19429=CARTESIAN_POINT('Origin',(1.5,-1.9,1.75));
#19430=CARTESIAN_POINT('',(1.29,-1.9,2.4));
#19431=CARTESIAN_POINT('',(1.29,-1.9,1.7));
#19432=CARTESIAN_POINT('Origin',(1.5,-1.9,2.4));
#19433=CARTESIAN_POINT('',(1.43596875762567,-1.7,1.75));
#19434=CARTESIAN_POINT('Origin',(1.5,-1.9,1.75));
#19435=CARTESIAN_POINT('',(1.43596875762567,-1.7,1.7));
#19436=CARTESIAN_POINT('Origin',(-1.5,1.9,1.7));
#19437=CARTESIAN_POINT('',(-1.56403124237433,1.7,1.7));
#19438=CARTESIAN_POINT('',(-1.43596875762567,1.7,1.7));
#19439=CARTESIAN_POINT('',(-0.75,1.7,1.7));
#19440=CARTESIAN_POINT('Origin',(-1.5,1.9,1.7));
#19441=CARTESIAN_POINT('Origin',(-1.5,1.9,1.7));
#19442=CARTESIAN_POINT('',(-1.56403124237433,1.7,1.75));
#19443=CARTESIAN_POINT('',(-1.56403124237433,1.7,1.7));
#19444=CARTESIAN_POINT('',(-1.71,1.9,1.75));
#19445=CARTESIAN_POINT('Origin',(-1.5,1.9,1.75));
#19446=CARTESIAN_POINT('',(-1.71,1.9,2.4));
#19447=CARTESIAN_POINT('',(-1.71,1.9,1.7));
#19448=CARTESIAN_POINT('Origin',(-1.5,1.9,2.4));
#19449=CARTESIAN_POINT('',(-1.43596875762567,1.7,1.75));
#19450=CARTESIAN_POINT('Origin',(-1.5,1.9,1.75));
#19451=CARTESIAN_POINT('',(-1.43596875762567,1.7,1.7));
#19452=CARTESIAN_POINT('Origin',(-1.5,-1.9,1.7));
#19453=CARTESIAN_POINT('',(-1.43596875762567,-1.7,1.7));
#19454=CARTESIAN_POINT('',(-1.56403124237433,-1.7,1.7));
#19455=CARTESIAN_POINT('',(-0.75,-1.7,1.7));
#19456=CARTESIAN_POINT('Origin',(-1.5,-1.9,1.7));
#19457=CARTESIAN_POINT('Origin',(-1.5,-1.9,1.7));
#19458=CARTESIAN_POINT('',(-1.43596875762567,-1.7,1.75));
#19459=CARTESIAN_POINT('',(-1.43596875762567,-1.7,1.7));
#19460=CARTESIAN_POINT('',(-1.71,-1.9,1.75));
#19461=CARTESIAN_POINT('Origin',(-1.5,-1.9,1.75));
#19462=CARTESIAN_POINT('',(-1.71,-1.9,2.4));
#19463=CARTESIAN_POINT('',(-1.71,-1.9,1.7));
#19464=CARTESIAN_POINT('Origin',(-1.5,-1.9,2.4));
#19465=CARTESIAN_POINT('',(-1.56403124237433,-1.7,1.75));
#19466=CARTESIAN_POINT('Origin',(-1.5,-1.9,1.75));
#19467=CARTESIAN_POINT('',(-1.56403124237433,-1.7,1.7));
#19468=CARTESIAN_POINT('Origin',(1.5,1.9,1.7));
#19469=CARTESIAN_POINT('',(1.43596875762567,1.7,1.7));
#19470=CARTESIAN_POINT('',(1.56403124237433,1.7,1.7));
#19471=CARTESIAN_POINT('',(0.75,1.7,1.7));
#19472=CARTESIAN_POINT('Origin',(1.5,1.9,1.7));
#19473=CARTESIAN_POINT('Origin',(1.5,1.9,1.7));
#19474=CARTESIAN_POINT('',(1.43596875762567,1.7,1.75));
#19475=CARTESIAN_POINT('',(1.43596875762567,1.7,1.7));
#19476=CARTESIAN_POINT('',(1.29,1.9,1.75));
#19477=CARTESIAN_POINT('Origin',(1.5,1.9,1.75));
#19478=CARTESIAN_POINT('',(1.29,1.9,2.4));
#19479=CARTESIAN_POINT('',(1.29,1.9,1.7));
#19480=CARTESIAN_POINT('Origin',(1.5,1.9,2.4));
#19481=CARTESIAN_POINT('',(1.56403124237433,1.7,1.75));
#19482=CARTESIAN_POINT('Origin',(1.5,1.9,1.75));
#19483=CARTESIAN_POINT('',(1.56403124237433,1.7,1.7));
#19484=CARTESIAN_POINT('Origin',(0.,-1.7,1.75));
#19485=CARTESIAN_POINT('',(0.,-1.7,1.75));
#19486=CARTESIAN_POINT('',(-1.97,-1.7,1.75));
#19487=CARTESIAN_POINT('',(0.,-1.7,1.75));
#19488=CARTESIAN_POINT('',(-1.97,-1.7,0.43));
#19489=CARTESIAN_POINT('',(-1.97,-1.7,1.75));
#19490=CARTESIAN_POINT('',(1.97,-1.7,0.43));
#19491=CARTESIAN_POINT('',(0.,-1.7,0.43));
#19492=CARTESIAN_POINT('',(1.97,-1.7,1.75));
#19493=CARTESIAN_POINT('',(1.97,-1.7,1.75));
#19494=CARTESIAN_POINT('',(0.,-1.7,1.75));
#19495=CARTESIAN_POINT('Origin',(0.,1.7,0.43));
#19496=CARTESIAN_POINT('',(0.,1.7,1.75));
#19497=CARTESIAN_POINT('',(1.97,1.7,1.75));
#19498=CARTESIAN_POINT('',(0.,1.7,1.75));
#19499=CARTESIAN_POINT('',(1.97,1.7,0.43));
#19500=CARTESIAN_POINT('',(1.97,1.7,0.43));
#19501=CARTESIAN_POINT('',(-1.97,1.7,0.43));
#19502=CARTESIAN_POINT('',(0.,1.7,0.43));
#19503=CARTESIAN_POINT('',(-1.97,1.7,1.75));
#19504=CARTESIAN_POINT('',(-1.97,1.7,0.43));
#19505=CARTESIAN_POINT('',(0.,1.7,1.75));
#19506=CARTESIAN_POINT('Origin',(-1.97,0.,1.415));
#19507=CARTESIAN_POINT('',(-1.97,-2.35,1.75));
#19508=CARTESIAN_POINT('',(-1.97,-2.35,1.75));
#19509=CARTESIAN_POINT('',(-1.97,-2.35,2.4));
#19510=CARTESIAN_POINT('',(-1.97,-2.35,2.4));
#19511=CARTESIAN_POINT('',(-1.97,2.35,2.4));
#19512=CARTESIAN_POINT('',(-1.97,2.35,2.4));
#19513=CARTESIAN_POINT('',(-1.97,2.35,1.75));
#19514=CARTESIAN_POINT('',(-1.97,2.35,1.75));
#19515=CARTESIAN_POINT('',(-1.97,1.7,1.75));
#19516=CARTESIAN_POINT('',(-1.97,0.78,0.43));
#19517=CARTESIAN_POINT('',(-1.97,0.78,0.43));
#19518=CARTESIAN_POINT('',(-1.97,0.78,1.55));
#19519=CARTESIAN_POINT('',(-1.97,0.78,1.55));
#19520=CARTESIAN_POINT('',(-1.97,-0.78,1.55));
#19521=CARTESIAN_POINT('',(-1.97,-0.78,1.55));
#19522=CARTESIAN_POINT('',(-1.97,-0.78,0.43));
#19523=CARTESIAN_POINT('',(-1.97,-0.78,0.43));
#19524=CARTESIAN_POINT('',(-1.97,-1.7,0.43));
#19525=CARTESIAN_POINT('Origin',(0.,-2.35,1.75));
#19526=CARTESIAN_POINT('',(1.97,-2.35,1.75));
#19527=CARTESIAN_POINT('',(1.97,-2.35,1.75));
#19528=CARTESIAN_POINT('',(0.,-2.35,1.75));
#19529=CARTESIAN_POINT('Origin',(0.,-2.35,2.4));
#19530=CARTESIAN_POINT('',(1.97,-2.35,2.4));
#19531=CARTESIAN_POINT('',(1.97,-2.35,2.4));
#19532=CARTESIAN_POINT('',(0.,-2.35,2.4));
#19533=CARTESIAN_POINT('Origin',(0.,2.35,2.4));
#19534=CARTESIAN_POINT('',(1.97,2.35,2.4));
#19535=CARTESIAN_POINT('',(1.97,2.35,2.4));
#19536=CARTESIAN_POINT('',(0.,2.35,2.4));
#19537=CARTESIAN_POINT('Origin',(0.,2.35,1.75));
#19538=CARTESIAN_POINT('',(1.97,2.35,1.75));
#19539=CARTESIAN_POINT('',(1.97,2.35,1.75));
#19540=CARTESIAN_POINT('',(0.,2.35,1.75));
#19541=CARTESIAN_POINT('Origin',(0.,1.7,1.75));
#19542=CARTESIAN_POINT('',(1.97,1.7,1.75));
#19543=CARTESIAN_POINT('Origin',(0.,0.78,0.43));
#19544=CARTESIAN_POINT('',(1.97,0.78,0.43));
#19545=CARTESIAN_POINT('',(1.97,0.78,0.43));
#19546=CARTESIAN_POINT('',(0.,0.78,0.43));
#19547=CARTESIAN_POINT('Origin',(0.,0.78,1.55));
#19548=CARTESIAN_POINT('',(1.97,0.78,1.55));
#19549=CARTESIAN_POINT('',(1.97,0.78,1.55));
#19550=CARTESIAN_POINT('',(0.,0.78,1.55));
#19551=CARTESIAN_POINT('Origin',(0.,-0.78,1.55));
#19552=CARTESIAN_POINT('',(1.97,-0.78,1.55));
#19553=CARTESIAN_POINT('',(1.97,-0.78,1.55));
#19554=CARTESIAN_POINT('',(0.,-0.78,1.55));
#19555=CARTESIAN_POINT('Origin',(0.,-0.78,0.43));
#19556=CARTESIAN_POINT('',(1.97,-0.78,0.43));
#19557=CARTESIAN_POINT('',(1.97,-0.78,0.43));
#19558=CARTESIAN_POINT('',(0.,-0.78,0.43));
#19559=CARTESIAN_POINT('Origin',(0.,-1.7,0.43));
#19560=CARTESIAN_POINT('',(1.97,-1.7,0.43));
#19561=CARTESIAN_POINT('Origin',(1.97,0.,1.415));
#19562=CARTESIAN_POINT('',(0.,0.,0.));
#19563=CARTESIAN_POINT('Origin',(1.97,1.7,2.3));
#19564=CARTESIAN_POINT('',(1.97,1.7,2.3));
#19565=CARTESIAN_POINT('',(1.97,-1.7,2.3));
#19566=CARTESIAN_POINT('',(1.97,1.7,2.3));
#19567=CARTESIAN_POINT('',(3.07,-1.7,2.3));
#19568=CARTESIAN_POINT('',(1.97,-1.7,2.3));
#19569=CARTESIAN_POINT('',(3.07,1.7,2.3));
#19570=CARTESIAN_POINT('',(3.07,1.7,2.3));
#19571=CARTESIAN_POINT('',(1.97,1.7,2.3));
#19572=CARTESIAN_POINT('Origin',(1.97,1.7,0.46));
#19573=CARTESIAN_POINT('',(1.97,1.7,0.46));
#19574=CARTESIAN_POINT('',(1.97,1.7,0.46));
#19575=CARTESIAN_POINT('',(3.07,1.7,0.46));
#19576=CARTESIAN_POINT('',(3.07,1.7,0.46));
#19577=CARTESIAN_POINT('',(1.97,1.7,0.46));
#19578=CARTESIAN_POINT('Origin',(1.97,0.78,0.46));
#19579=CARTESIAN_POINT('',(1.97,0.78,0.46));
#19580=CARTESIAN_POINT('',(1.97,0.78,0.46));
#19581=CARTESIAN_POINT('',(3.07,0.78,0.46));
#19582=CARTESIAN_POINT('',(3.07,0.78,0.46));
#19583=CARTESIAN_POINT('',(1.97,0.78,0.46));
#19584=CARTESIAN_POINT('Origin',(1.97,0.78,1.55));
#19585=CARTESIAN_POINT('',(1.97,0.78,1.55));
#19586=CARTESIAN_POINT('',(1.97,0.78,1.55));
#19587=CARTESIAN_POINT('',(3.07,0.78,1.55));
#19588=CARTESIAN_POINT('',(3.07,0.78,1.55));
#19589=CARTESIAN_POINT('',(1.97,0.78,1.55));
#19590=CARTESIAN_POINT('Origin',(1.97,-0.78,1.55));
#19591=CARTESIAN_POINT('',(1.97,-0.78,1.55));
#19592=CARTESIAN_POINT('',(1.97,-0.78,1.55));
#19593=CARTESIAN_POINT('',(3.07,-0.78,1.55));
#19594=CARTESIAN_POINT('',(3.07,-0.78,1.55));
#19595=CARTESIAN_POINT('',(1.97,-0.78,1.55));
#19596=CARTESIAN_POINT('Origin',(1.97,-0.78,0.46));
#19597=CARTESIAN_POINT('',(1.97,-0.78,0.46));
#19598=CARTESIAN_POINT('',(1.97,-0.78,0.46));
#19599=CARTESIAN_POINT('',(3.07,-0.78,0.46));
#19600=CARTESIAN_POINT('',(3.07,-0.78,0.46));
#19601=CARTESIAN_POINT('',(1.97,-0.78,0.46));
#19602=CARTESIAN_POINT('Origin',(1.97,-1.7,0.46));
#19603=CARTESIAN_POINT('',(1.97,-1.7,0.46));
#19604=CARTESIAN_POINT('',(1.97,-1.7,0.46));
#19605=CARTESIAN_POINT('',(3.07,-1.7,0.46));
#19606=CARTESIAN_POINT('',(3.07,-1.7,0.46));
#19607=CARTESIAN_POINT('',(1.97,-1.7,0.46));
#19608=CARTESIAN_POINT('Origin',(1.97,-1.7,2.3));
#19609=CARTESIAN_POINT('',(1.97,-1.7,2.3));
#19610=CARTESIAN_POINT('',(3.07,-1.7,2.3));
#19611=CARTESIAN_POINT('Origin',(3.07,0.,1.38));
#19612=CARTESIAN_POINT('Origin',(1.97,0.,1.38));
#19613=CARTESIAN_POINT('',(0.,0.,0.));
#19614=CARTESIAN_POINT('Origin',(-1.97,-0.78,0.46));
#19615=CARTESIAN_POINT('',(-1.97,-1.7,0.46));
#19616=CARTESIAN_POINT('',(-1.97,-0.78,0.46));
#19617=CARTESIAN_POINT('',(-1.97,-1.7,0.46));
#19618=CARTESIAN_POINT('',(-3.07,-1.7,0.46));
#19619=CARTESIAN_POINT('',(-1.97,-1.7,0.46));
#19620=CARTESIAN_POINT('',(-3.07,-0.78,0.46));
#19621=CARTESIAN_POINT('',(-3.07,-1.7,0.46));
#19622=CARTESIAN_POINT('',(-1.97,-0.78,0.46));
#19623=CARTESIAN_POINT('Origin',(-1.97,-0.78,1.55));
#19624=CARTESIAN_POINT('',(-1.97,-0.78,1.55));
#19625=CARTESIAN_POINT('',(-1.97,-0.78,0.46));
#19626=CARTESIAN_POINT('',(-3.07,-0.78,1.55));
#19627=CARTESIAN_POINT('',(-3.07,-0.78,0.46));
#19628=CARTESIAN_POINT('',(-1.97,-0.78,1.55));
#19629=CARTESIAN_POINT('Origin',(-1.97,0.78,1.55));
#19630=CARTESIAN_POINT('',(-1.97,0.78,1.55));
#19631=CARTESIAN_POINT('',(-1.97,-0.78,1.55));
#19632=CARTESIAN_POINT('',(-3.07,0.78,1.55));
#19633=CARTESIAN_POINT('',(-3.07,-0.78,1.55));
#19634=CARTESIAN_POINT('',(-1.97,0.78,1.55));
#19635=CARTESIAN_POINT('Origin',(-1.97,0.78,0.46));
#19636=CARTESIAN_POINT('',(-1.97,0.78,0.46));
#19637=CARTESIAN_POINT('',(-1.97,0.78,1.55));
#19638=CARTESIAN_POINT('',(-3.07,0.78,0.46));
#19639=CARTESIAN_POINT('',(-3.07,0.78,1.55));
#19640=CARTESIAN_POINT('',(-1.97,0.78,0.46));
#19641=CARTESIAN_POINT('Origin',(-1.97,1.7,0.46));
#19642=CARTESIAN_POINT('',(-1.97,1.7,0.46));
#19643=CARTESIAN_POINT('',(-1.97,0.78,0.46));
#19644=CARTESIAN_POINT('',(-3.07,1.7,0.46));
#19645=CARTESIAN_POINT('',(-3.07,0.78,0.46));
#19646=CARTESIAN_POINT('',(-1.97,1.7,0.46));
#19647=CARTESIAN_POINT('Origin',(-1.97,1.7,2.3));
#19648=CARTESIAN_POINT('',(-1.97,1.7,2.3));
#19649=CARTESIAN_POINT('',(-1.97,1.7,0.46));
#19650=CARTESIAN_POINT('',(-3.07,1.7,2.3));
#19651=CARTESIAN_POINT('',(-3.07,1.7,0.46));
#19652=CARTESIAN_POINT('',(-1.97,1.7,2.3));
#19653=CARTESIAN_POINT('Origin',(-1.97,-1.7,2.3));
#19654=CARTESIAN_POINT('',(-1.97,-1.7,2.3));
#19655=CARTESIAN_POINT('',(-1.97,1.7,2.3));
#19656=CARTESIAN_POINT('',(-3.07,-1.7,2.3));
#19657=CARTESIAN_POINT('',(-3.07,1.7,2.3));
#19658=CARTESIAN_POINT('',(-1.97,-1.7,2.3));
#19659=CARTESIAN_POINT('Origin',(-1.97,-1.7,0.46));
#19660=CARTESIAN_POINT('',(-1.97,-1.7,2.3));
#19661=CARTESIAN_POINT('',(-3.07,-1.7,2.3));
#19662=CARTESIAN_POINT('Origin',(-1.97,0.,1.38));
#19663=CARTESIAN_POINT('Origin',(-3.07,0.,1.38));
#19664=CARTESIAN_POINT('',(0.,0.,0.));
#19665=CARTESIAN_POINT('',(0.,0.,0.));
#19666=CARTESIAN_POINT('',(0.,0.,0.));
#19667=CARTESIAN_POINT('',(0.,0.,0.));
#19668=CARTESIAN_POINT('Origin',(0.,0.09,0.));
#19669=CARTESIAN_POINT('',(-0.285,0.1,3.49024337756996E-17));
#19670=CARTESIAN_POINT('Origin',(0.,0.1,0.));
#19671=CARTESIAN_POINT('',(-0.265,0.08,-3.24531401774049E-17));
#19672=CARTESIAN_POINT('',(-0.275,0.09,3.36777869765522E-17));
#19673=CARTESIAN_POINT('Origin',(0.,0.08,0.));
#19674=CARTESIAN_POINT('Origin',(0.,0.,0.));
#19675=CARTESIAN_POINT('',(-0.265,0.,3.24531401774049E-17));
#19676=CARTESIAN_POINT('',(-0.265,0.,3.24531401774049E-17));
#19677=CARTESIAN_POINT('Origin',(0.,0.,0.));
#19678=CARTESIAN_POINT('Origin',(0.,0.1,0.));
#19679=CARTESIAN_POINT('',(-0.5,0.1,6.12323399573677E-17));
#19680=CARTESIAN_POINT('Origin',(0.,0.1,0.));
#19681=CARTESIAN_POINT('Origin',(0.,0.,0.));
#19682=CARTESIAN_POINT('',(-0.5,0.,6.12323399573677E-17));
#19683=CARTESIAN_POINT('',(-0.5,0.,6.12323399573677E-17));
#19684=CARTESIAN_POINT('Origin',(0.,0.,0.));
#19685=CARTESIAN_POINT('Origin',(0.,0.,0.));
#19686=CARTESIAN_POINT('',(0.,0.,0.));
#19687=CARTESIAN_POINT('Origin',(0.375,0.5,0.));
#19688=CARTESIAN_POINT('',(-0.375,0.5,-4.59242549680257E-17));
#19689=CARTESIAN_POINT('Origin',(0.,0.5,0.));
#19690=CARTESIAN_POINT('Origin',(0.,0.475,0.));
#19691=CARTESIAN_POINT('',(-0.425,0.45,-5.20474889637625E-17));
#19692=CARTESIAN_POINT('Origin',(0.,0.45,0.));
#19693=CARTESIAN_POINT('',(-0.4,0.475,-4.89858719658941E-17));
#19694=CARTESIAN_POINT('Origin',(0.,0.24,0.));
#19695=CARTESIAN_POINT('',(-0.425,0.0299999999999998,-5.20474889637625E-17));
#19696=CARTESIAN_POINT('Origin',(0.,0.0299999999999998,0.));
#19697=CARTESIAN_POINT('',(-0.425,0.24,-5.20474889637625E-17));
#19698=CARTESIAN_POINT('Origin',(0.,0.0150000000000001,0.));
#19699=CARTESIAN_POINT('',(-0.395,4.85722573273506E-17,-4.83735485663204E-17));
#19700=CARTESIAN_POINT('Origin',(0.,0.,0.));
#19701=CARTESIAN_POINT('',(-0.41,0.0150000000000001,-5.02105187650415E-17));
#19702=CARTESIAN_POINT('Origin',(0.27,0.,0.));
#19703=CARTESIAN_POINT('',(-0.27,0.,-3.30654635769785E-17));
#19704=CARTESIAN_POINT('Origin',(0.,0.,0.));
#19705=CARTESIAN_POINT('Origin',(0.,-0.02,0.));
#19706=CARTESIAN_POINT('',(-0.24505,-0.0498999999999999,3.00099698131059E-17));
#19707=CARTESIAN_POINT('Origin',(0.,-0.0498999999999999,0.));
#19708=CARTESIAN_POINT('',(-0.26,-0.02,-3.18408167778312E-17));
#19709=CARTESIAN_POINT('Origin',(0.,-0.995,0.));
#19710=CARTESIAN_POINT('',(-0.24505,-1.95495,3.00099698131059E-17));
#19711=CARTESIAN_POINT('Origin',(0.,-1.95495,0.));
#19712=CARTESIAN_POINT('',(-0.24505,-0.995,-3.00099698131059E-17));
#19713=CARTESIAN_POINT('Origin',(0.,-1.975,0.));
#19714=CARTESIAN_POINT('',(-0.2,-2.,-2.44929359829471E-17));
#19715=CARTESIAN_POINT('Origin',(0.,-2.,0.));
#19716=CARTESIAN_POINT('',(-0.225,-1.975,-2.75545529808154E-17));
#19717=CARTESIAN_POINT('Origin',(0.,-2.,0.));
#19718=CARTESIAN_POINT('Origin',(0.115470053837925,-0.5,-0.2));
#19719=CARTESIAN_POINT('',(0.23094010767585,-0.5,0.));
#19720=CARTESIAN_POINT('',(0.115470053837925,-0.5,-0.2));
#19721=CARTESIAN_POINT('',(0.23094010767585,-0.5,0.));
#19722=CARTESIAN_POINT('',(0.115470053837925,-0.8,-0.2));
#19723=CARTESIAN_POINT('',(0.115470053837925,-0.5,-0.2));
#19724=CARTESIAN_POINT('',(0.23094010767585,-0.8,0.));
#19725=CARTESIAN_POINT('',(0.23094010767585,-0.8,0.));
#19726=CARTESIAN_POINT('',(0.23094010767585,-0.5,0.));
#19727=CARTESIAN_POINT('Origin',(-0.115470053837925,-0.5,-0.2));
#19728=CARTESIAN_POINT('',(-0.115470053837925,-0.5,-0.2));
#19729=CARTESIAN_POINT('',(0.115470053837925,-0.5,-0.2));
#19730=CARTESIAN_POINT('',(-0.115470053837925,-0.8,-0.2));
#19731=CARTESIAN_POINT('',(-0.115470053837925,-0.5,-0.2));
#19732=CARTESIAN_POINT('',(0.115470053837925,-0.8,-0.2));
#19733=CARTESIAN_POINT('Origin',(-0.23094010767585,-0.5,-2.77555756156289E-17));
#19734=CARTESIAN_POINT('',(-0.23094010767585,-0.5,-2.82820063659975E-17));
#19735=CARTESIAN_POINT('',(-0.115470053837925,-0.5,-0.2));
#19736=CARTESIAN_POINT('',(-0.23094010767585,-0.8,-2.77555756156289E-17));
#19737=CARTESIAN_POINT('',(-0.23094010767585,-0.5,-2.82820063659975E-17));
#19738=CARTESIAN_POINT('',(-0.115470053837925,-0.8,-0.2));
#19739=CARTESIAN_POINT('Origin',(-0.115470053837925,-0.5,0.2));
#19740=CARTESIAN_POINT('',(-0.115470053837925,-0.5,0.2));
#19741=CARTESIAN_POINT('',(-0.23094010767585,-0.5,-2.82820063659975E-17));
#19742=CARTESIAN_POINT('',(-0.115470053837925,-0.8,0.2));
#19743=CARTESIAN_POINT('',(-0.115470053837925,-0.5,0.2));
#19744=CARTESIAN_POINT('',(-0.23094010767585,-0.8,-2.82820063659975E-17));
#19745=CARTESIAN_POINT('Origin',(0.115470053837925,-0.5,0.2));
#19746=CARTESIAN_POINT('',(0.115470053837925,-0.5,0.2));
#19747=CARTESIAN_POINT('',(-0.115470053837925,-0.5,0.2));
#19748=CARTESIAN_POINT('',(0.115470053837925,-0.8,0.2));
#19749=CARTESIAN_POINT('',(0.115470053837925,-0.5,0.2));
#19750=CARTESIAN_POINT('',(-0.115470053837925,-0.8,0.2));
#19751=CARTESIAN_POINT('Origin',(0.23094010767585,-0.5,0.));
#19752=CARTESIAN_POINT('',(0.115470053837925,-0.5,0.2));
#19753=CARTESIAN_POINT('',(0.115470053837925,-0.8,0.2));
#19754=CARTESIAN_POINT('Origin',(0.,-0.5,0.));
#19755=CARTESIAN_POINT('Origin',(0.,-0.8,0.));
#19756=CARTESIAN_POINT('',(0.,0.,0.));
#19757=CARTESIAN_POINT('Origin',(0.0866025403784439,-0.4,-0.15));
#19758=CARTESIAN_POINT('',(0.173205080756888,-0.4,0.));
#19759=CARTESIAN_POINT('',(0.0866025403784439,-0.4,-0.15));
#19760=CARTESIAN_POINT('',(0.173205080756888,-0.4,0.));
#19761=CARTESIAN_POINT('',(0.0866025403784439,-0.64,-0.15));
#19762=CARTESIAN_POINT('',(0.0866025403784439,-0.4,-0.15));
#19763=CARTESIAN_POINT('',(0.173205080756888,-0.64,0.));
#19764=CARTESIAN_POINT('',(0.173205080756888,-0.64,0.));
#19765=CARTESIAN_POINT('',(0.173205080756888,-0.4,0.));
#19766=CARTESIAN_POINT('Origin',(-0.0866025403784438,-0.4,-0.15));
#19767=CARTESIAN_POINT('',(-0.0866025403784438,-0.4,-0.15));
#19768=CARTESIAN_POINT('',(0.0866025403784439,-0.4,-0.15));
#19769=CARTESIAN_POINT('',(-0.0866025403784438,-0.64,-0.15));
#19770=CARTESIAN_POINT('',(-0.0866025403784438,-0.4,-0.15));
#19771=CARTESIAN_POINT('',(0.0866025403784439,-0.64,-0.15));
#19772=CARTESIAN_POINT('Origin',(-0.173205080756888,-0.4,-2.77555756156289E-17));
#19773=CARTESIAN_POINT('',(-0.173205080756888,-0.4,-2.12115047744981E-17));
#19774=CARTESIAN_POINT('',(-0.0866025403784438,-0.4,-0.15));
#19775=CARTESIAN_POINT('',(-0.173205080756888,-0.64,-2.77555756156289E-17));
#19776=CARTESIAN_POINT('',(-0.173205080756888,-0.4,-2.12115047744981E-17));
#19777=CARTESIAN_POINT('',(-0.0866025403784438,-0.64,-0.15));
#19778=CARTESIAN_POINT('Origin',(-0.0866025403784439,-0.4,0.15));
#19779=CARTESIAN_POINT('',(-0.0866025403784439,-0.4,0.15));
#19780=CARTESIAN_POINT('',(-0.173205080756888,-0.4,-2.12115047744981E-17));
#19781=CARTESIAN_POINT('',(-0.0866025403784439,-0.64,0.15));
#19782=CARTESIAN_POINT('',(-0.0866025403784439,-0.4,0.15));
#19783=CARTESIAN_POINT('',(-0.173205080756888,-0.64,-2.12115047744981E-17));
#19784=CARTESIAN_POINT('Origin',(0.0866025403784439,-0.4,0.15));
#19785=CARTESIAN_POINT('',(0.0866025403784439,-0.4,0.15));
#19786=CARTESIAN_POINT('',(-0.0866025403784439,-0.4,0.15));
#19787=CARTESIAN_POINT('',(0.0866025403784439,-0.64,0.15));
#19788=CARTESIAN_POINT('',(0.0866025403784439,-0.4,0.15));
#19789=CARTESIAN_POINT('',(-0.0866025403784439,-0.64,0.15));
#19790=CARTESIAN_POINT('Origin',(0.173205080756888,-0.4,0.));
#19791=CARTESIAN_POINT('',(0.0866025403784439,-0.4,0.15));
#19792=CARTESIAN_POINT('',(0.0866025403784439,-0.64,0.15));
#19793=CARTESIAN_POINT('Origin',(0.,-0.4,-2.77555756156289E-17));
#19794=CARTESIAN_POINT('Origin',(0.,-0.64,-2.77555756156289E-17));
#19795=CARTESIAN_POINT('Origin',(0.,-1.,0.));
#19796=CARTESIAN_POINT('',(-0.1954,-1.,2.39295984553393E-17));
#19797=CARTESIAN_POINT('Origin',(0.,-1.,0.));
#19798=CARTESIAN_POINT('Origin',(0.3,0.4,0.));
#19799=CARTESIAN_POINT('',(-0.3,0.4,-3.67394039744206E-17));
#19800=CARTESIAN_POINT('Origin',(0.,0.4,0.));
#19801=CARTESIAN_POINT('Origin',(0.,0.375,0.));
#19802=CARTESIAN_POINT('',(-0.35,0.35,-4.28626379701573E-17));
#19803=CARTESIAN_POINT('Origin',(0.,0.35,0.));
#19804=CARTESIAN_POINT('',(-0.325,0.375,-3.9801020972289E-17));
#19805=CARTESIAN_POINT('Origin',(0.,0.19,0.));
#19806=CARTESIAN_POINT('',(-0.35,0.03,-4.28626379701574E-17));
#19807=CARTESIAN_POINT('Origin',(0.,0.03,0.));
#19808=CARTESIAN_POINT('',(-0.35,0.19,-4.28626379701574E-17));
#19809=CARTESIAN_POINT('Origin',(0.,0.0149999999999999,0.));
#19810=CARTESIAN_POINT('',(-0.32,-3.29597460435593E-17,-3.91886975727153E-17));
#19811=CARTESIAN_POINT('Origin',(0.,0.,0.));
#19812=CARTESIAN_POINT('',(-0.335,0.0149999999999999,-4.10256677714363E-17));
#19813=CARTESIAN_POINT('Origin',(0.22,0.,0.));
#19814=CARTESIAN_POINT('',(-0.22,-6.93889390390723E-18,-2.69422295812418E-17));
#19815=CARTESIAN_POINT('Origin',(0.,0.,0.));
#19816=CARTESIAN_POINT('Origin',(0.,-0.02,0.));
#19817=CARTESIAN_POINT('',(-0.1954,-0.0492,2.39295984553393E-17));
#19818=CARTESIAN_POINT('Origin',(0.,-0.0492,0.));
#19819=CARTESIAN_POINT('',(-0.21,-0.02,-2.57175827820944E-17));
#19820=CARTESIAN_POINT('Origin',(0.,-0.8,0.));
#19821=CARTESIAN_POINT('',(-0.1954,-0.8,-2.39295984553393E-17));
#19822=CARTESIAN_POINT('',(0.,0.,0.));
#19823=CARTESIAN_POINT('Origin',(0.3,0.4,0.));
#19824=CARTESIAN_POINT('',(-0.3,0.4,-3.67394039744206E-17));
#19825=CARTESIAN_POINT('Origin',(0.,0.4,0.));
#19826=CARTESIAN_POINT('Origin',(0.,0.375,0.));
#19827=CARTESIAN_POINT('',(-0.35,0.35,-4.28626379701573E-17));
#19828=CARTESIAN_POINT('Origin',(0.,0.35,0.));
#19829=CARTESIAN_POINT('',(-0.325,0.375,-3.9801020972289E-17));
#19830=CARTESIAN_POINT('Origin',(0.,0.19,0.));
#19831=CARTESIAN_POINT('',(-0.35,0.03,-4.28626379701574E-17));
#19832=CARTESIAN_POINT('Origin',(0.,0.03,0.));
#19833=CARTESIAN_POINT('',(-0.35,0.19,-4.28626379701574E-17));
#19834=CARTESIAN_POINT('Origin',(0.,0.0149999999999999,0.));
#19835=CARTESIAN_POINT('',(-0.32,-3.29597460435593E-17,-3.91886975727153E-17));
#19836=CARTESIAN_POINT('Origin',(0.,0.,0.));
#19837=CARTESIAN_POINT('',(-0.335,0.0149999999999999,-4.10256677714363E-17));
#19838=CARTESIAN_POINT('Origin',(0.22,0.,0.));
#19839=CARTESIAN_POINT('',(-0.22,-6.93889390390723E-18,-2.69422295812418E-17));
#19840=CARTESIAN_POINT('Origin',(0.,0.,0.));
#19841=CARTESIAN_POINT('Origin',(0.,-0.02,0.));
#19842=CARTESIAN_POINT('',(-0.1954,-0.0492,2.39295984553393E-17));
#19843=CARTESIAN_POINT('Origin',(0.,-0.0492,0.));
#19844=CARTESIAN_POINT('',(-0.21,-0.02,-2.57175827820944E-17));
#19845=CARTESIAN_POINT('Origin',(0.,-0.8,0.));
#19846=CARTESIAN_POINT('',(-0.1954,-1.5646,2.39295984553393E-17));
#19847=CARTESIAN_POINT('Origin',(0.,-1.5646,0.));
#19848=CARTESIAN_POINT('',(-0.1954,-0.8,-2.39295984553393E-17));
#19849=CARTESIAN_POINT('Origin',(0.,-1.58,0.));
#19850=CARTESIAN_POINT('',(-0.16,-1.6,-1.95943487863577E-17));
#19851=CARTESIAN_POINT('Origin',(0.,-1.6,0.));
#19852=CARTESIAN_POINT('',(-0.18,-1.58,-2.20436423846524E-17));
#19853=CARTESIAN_POINT('Origin',(0.,-1.6,0.));
#19854=CARTESIAN_POINT('Origin',(0.0866025403784439,-0.4,-0.15));
#19855=CARTESIAN_POINT('',(0.173205080756888,-0.4,0.));
#19856=CARTESIAN_POINT('',(0.0866025403784439,-0.4,-0.15));
#19857=CARTESIAN_POINT('',(0.173205080756888,-0.4,0.));
#19858=CARTESIAN_POINT('',(0.0866025403784439,-0.64,-0.15));
#19859=CARTESIAN_POINT('',(0.0866025403784439,-0.4,-0.15));
#19860=CARTESIAN_POINT('',(0.173205080756888,-0.64,0.));
#19861=CARTESIAN_POINT('',(0.173205080756888,-0.64,0.));
#19862=CARTESIAN_POINT('',(0.173205080756888,-0.4,0.));
#19863=CARTESIAN_POINT('Origin',(-0.0866025403784438,-0.4,-0.15));
#19864=CARTESIAN_POINT('',(-0.0866025403784438,-0.4,-0.15));
#19865=CARTESIAN_POINT('',(0.0866025403784439,-0.4,-0.15));
#19866=CARTESIAN_POINT('',(-0.0866025403784438,-0.64,-0.15));
#19867=CARTESIAN_POINT('',(-0.0866025403784438,-0.4,-0.15));
#19868=CARTESIAN_POINT('',(0.0866025403784439,-0.64,-0.15));
#19869=CARTESIAN_POINT('Origin',(-0.173205080756888,-0.4,-2.77555756156289E-17));
#19870=CARTESIAN_POINT('',(-0.173205080756888,-0.4,-2.12115047744981E-17));
#19871=CARTESIAN_POINT('',(-0.0866025403784438,-0.4,-0.15));
#19872=CARTESIAN_POINT('',(-0.173205080756888,-0.64,-2.77555756156289E-17));
#19873=CARTESIAN_POINT('',(-0.173205080756888,-0.4,-2.12115047744981E-17));
#19874=CARTESIAN_POINT('',(-0.0866025403784438,-0.64,-0.15));
#19875=CARTESIAN_POINT('Origin',(-0.0866025403784439,-0.4,0.15));
#19876=CARTESIAN_POINT('',(-0.0866025403784439,-0.4,0.15));
#19877=CARTESIAN_POINT('',(-0.173205080756888,-0.4,-2.12115047744981E-17));
#19878=CARTESIAN_POINT('',(-0.0866025403784439,-0.64,0.15));
#19879=CARTESIAN_POINT('',(-0.0866025403784439,-0.4,0.15));
#19880=CARTESIAN_POINT('',(-0.173205080756888,-0.64,-2.12115047744981E-17));
#19881=CARTESIAN_POINT('Origin',(0.0866025403784439,-0.4,0.15));
#19882=CARTESIAN_POINT('',(0.0866025403784439,-0.4,0.15));
#19883=CARTESIAN_POINT('',(-0.0866025403784439,-0.4,0.15));
#19884=CARTESIAN_POINT('',(0.0866025403784439,-0.64,0.15));
#19885=CARTESIAN_POINT('',(0.0866025403784439,-0.4,0.15));
#19886=CARTESIAN_POINT('',(-0.0866025403784439,-0.64,0.15));
#19887=CARTESIAN_POINT('Origin',(0.173205080756888,-0.4,0.));
#19888=CARTESIAN_POINT('',(0.0866025403784439,-0.4,0.15));
#19889=CARTESIAN_POINT('',(0.0866025403784439,-0.64,0.15));
#19890=CARTESIAN_POINT('Origin',(0.,-0.4,-2.77555756156289E-17));
#19891=CARTESIAN_POINT('Origin',(0.,-0.64,-2.77555756156289E-17));
#19892=CARTESIAN_POINT('',(0.,0.,0.));
#19893=CARTESIAN_POINT('',(0.,0.,0.));
#19894=CARTESIAN_POINT('',(0.,0.,0.));
#19895=CARTESIAN_POINT('',(0.,0.,0.));
#19896=CARTESIAN_POINT('',(0.,0.,0.));
#19897=CARTESIAN_POINT('',(0.,0.,0.));
#19898=CARTESIAN_POINT('',(0.,0.,0.));
#19899=CARTESIAN_POINT('',(0.,0.,0.));
#19900=CARTESIAN_POINT('',(0.,0.,0.));
#19901=CARTESIAN_POINT('',(0.,0.,0.));
#19902=CARTESIAN_POINT('',(0.,0.,0.));
#19903=CARTESIAN_POINT('',(0.,0.,0.));
#19904=CARTESIAN_POINT('',(0.,0.,0.));
#19905=CARTESIAN_POINT('',(0.,0.,0.));
#19906=CARTESIAN_POINT('',(-2.8,-1.,0.8));
#19907=CARTESIAN_POINT('',(-2.8,1.,0.8));
#19908=CARTESIAN_POINT('',(2.8,-1.,0.8));
#19909=CARTESIAN_POINT('',(2.8,1.,0.8));
#19910=CARTESIAN_POINT('',(0.,-0.9,7.));
#19911=CARTESIAN_POINT('',(0.,0.9,7.));
#19912=CARTESIAN_POINT('',(1.34350288425444,-2.1,8.34350288425444));
#19913=CARTESIAN_POINT('',(-1.34350288425444,-2.1,8.34350288425444));
#19914=CARTESIAN_POINT('',(-1.34350288425444,-2.1,5.65649711574556));
#19915=CARTESIAN_POINT('',(1.34350288425444,-2.1,5.65649711574556));
#19916=CARTESIAN_POINT('',(1.34350288425444,2.1,8.34350288425444));
#19917=CARTESIAN_POINT('',(-1.34350288425444,2.1,8.34350288425444));
#19918=CARTESIAN_POINT('',(-1.34350288425444,2.1,5.65649711574556));
#19919=CARTESIAN_POINT('',(1.34350288425444,2.1,5.65649711574556));
#19920=CARTESIAN_POINT('',(29.2,-1.,0.8));
#19921=CARTESIAN_POINT('',(29.2,1.,0.8));
#19922=CARTESIAN_POINT('',(34.8,-1.,0.8));
#19923=CARTESIAN_POINT('',(34.8,1.,0.8));
#19924=CARTESIAN_POINT('',(32.,-0.9,7.));
#19925=CARTESIAN_POINT('',(32.,0.9,7.));
#19926=CARTESIAN_POINT('',(33.3435028842544,-2.1,8.34350288425444));
#19927=CARTESIAN_POINT('',(30.6564971157456,-2.1,8.34350288425444));
#19928=CARTESIAN_POINT('',(30.6564971157456,-2.1,5.65649711574556));
#19929=CARTESIAN_POINT('',(33.3435028842544,-2.1,5.65649711574556));
#19930=CARTESIAN_POINT('',(33.3435028842544,2.1,8.34350288425444));
#19931=CARTESIAN_POINT('',(30.6564971157456,2.1,8.34350288425444));
#19932=CARTESIAN_POINT('',(30.6564971157456,2.1,5.65649711574556));
#19933=CARTESIAN_POINT('',(33.3435028842544,2.1,5.65649711574556));
#19934=CARTESIAN_POINT('',(-4.,-3.5,-2.2));
#19935=CARTESIAN_POINT('',(5.,-3.5,-1.78));
#19936=CARTESIAN_POINT('',(5.,-3.5,0.));
#19937=CARTESIAN_POINT('',(27.,-3.5,-1.78));
#19938=CARTESIAN_POINT('',(27.,-3.5,0.));
#19939=CARTESIAN_POINT('',(-4.,3.5,-2.2));
#19940=CARTESIAN_POINT('',(5.,3.5,-1.78));
#19941=CARTESIAN_POINT('',(5.,3.5,0.));
#19942=CARTESIAN_POINT('',(27.,3.5,-1.78));
#19943=CARTESIAN_POINT('',(27.,3.5,0.));
#19944=CARTESIAN_POINT('',(5.,0.,0.));
#19945=CARTESIAN_POINT('',(7.,0.,0.97));
#19946=CARTESIAN_POINT('',(13.,0.,0.97));
#19947=CARTESIAN_POINT('',(19.,0.,0.97));
#19948=CARTESIAN_POINT('',(25.,0.,0.97));
#19949=CARTESIAN_POINT('',(5.8,-2.5,0.8));
#19950=CARTESIAN_POINT('',(5.8,2.5,0.8));
#19951=CARTESIAN_POINT('',(26.2,-2.5,0.8));
#19952=CARTESIAN_POINT('',(26.2,2.5,0.8));
#19953=CARTESIAN_POINT('',(0.,0.,0.));
#19954=CARTESIAN_POINT('',(0.,0.,0.));
#19955=CARTESIAN_POINT('',(0.,0.,0.));
#19956=CARTESIAN_POINT('',(0.,0.,0.));
#19957=CARTESIAN_POINT('',(0.,0.,0.));
#19958=CARTESIAN_POINT('',(0.,0.,0.));
#19959=CARTESIAN_POINT('',(0.,-3.5,7.));
#19960=CARTESIAN_POINT('',(0.,-5.2,7.));
#19961=CARTESIAN_POINT('',(0.,0.,0.));
#19962=CARTESIAN_POINT('',(0.,0.,0.));
#19963=CARTESIAN_POINT('',(0.,0.,0.));
#19964=CARTESIAN_POINT('',(0.,0.,0.));
#19965=CARTESIAN_POINT('',(0.,0.,0.));
#19966=CARTESIAN_POINT('',(0.,0.,0.));
#19967=CARTESIAN_POINT('',(32.,-3.5,7.));
#19968=CARTESIAN_POINT('',(32.,-5.2,7.));
#19969=CARTESIAN_POINT('',(0.,0.,0.));
#19970=CARTESIAN_POINT('',(0.,0.,0.));
#19971=CARTESIAN_POINT('',(0.,0.,0.));
#19972=CARTESIAN_POINT('',(16.,0.,0.));
#19973=CARTESIAN_POINT('',(14.5,-1.9,3.6));
#19974=CARTESIAN_POINT('',(14.5,-1.9,3.7));
#19975=CARTESIAN_POINT('',(14.5,1.9,3.6));
#19976=CARTESIAN_POINT('',(14.5,1.9,3.7));
#19977=CARTESIAN_POINT('',(17.5,-1.9,3.6));
#19978=CARTESIAN_POINT('',(17.5,-1.9,3.7));
#19979=CARTESIAN_POINT('',(17.5,1.9,3.6));
#19980=CARTESIAN_POINT('',(17.5,1.9,3.7));
#19981=CARTESIAN_POINT('',(15.5,-1.8,8.13661977236758));
#19982=CARTESIAN_POINT('',(16.5,-1.8,8.13661977236758));
#19983=CARTESIAN_POINT('',(15.5,-1.8,2.8));
#19984=CARTESIAN_POINT('',(16.5,-1.8,2.8));
#19985=CARTESIAN_POINT('',(0.,0.,0.));
#19986=CARTESIAN_POINT('',(0.,0.,0.));
#19987=CARTESIAN_POINT('',(0.,0.,0.));
#19988=CARTESIAN_POINT('',(0.,0.,0.));
#19989=UNCERTAINTY_MEASURE_WITH_UNIT(LENGTH_MEASURE(0.001),#20097,
'DISTANCE_ACCURACY_VALUE',
'Maximum model space distance between geometric entities at asserted c
onnectivities');
#19990=UNCERTAINTY_MEASURE_WITH_UNIT(LENGTH_MEASURE(0.001),#20097,
'DISTANCE_ACCURACY_VALUE',
'Maximum model space distance between geometric entities at asserted c
onnectivities');
#19991=UNCERTAINTY_MEASURE_WITH_UNIT(LENGTH_MEASURE(0.001),#20097,
'DISTANCE_ACCURACY_VALUE',
'Maximum model space distance between geometric entities at asserted c
onnectivities');
#19992=UNCERTAINTY_MEASURE_WITH_UNIT(LENGTH_MEASURE(0.001),#20097,
'DISTANCE_ACCURACY_VALUE',
'Maximum model space distance between geometric entities at asserted c
onnectivities');
#19993=UNCERTAINTY_MEASURE_WITH_UNIT(LENGTH_MEASURE(0.001),#20097,
'DISTANCE_ACCURACY_VALUE',
'Maximum model space distance between geometric entities at asserted c
onnectivities');
#19994=UNCERTAINTY_MEASURE_WITH_UNIT(LENGTH_MEASURE(0.001),#20097,
'DISTANCE_ACCURACY_VALUE',
'Maximum model space distance between geometric entities at asserted c
onnectivities');
#19995=UNCERTAINTY_MEASURE_WITH_UNIT(LENGTH_MEASURE(0.001),#20097,
'DISTANCE_ACCURACY_VALUE',
'Maximum model space distance between geometric entities at asserted c
onnectivities');
#19996=UNCERTAINTY_MEASURE_WITH_UNIT(LENGTH_MEASURE(0.001),#20097,
'DISTANCE_ACCURACY_VALUE',
'Maximum model space distance between geometric entities at asserted c
onnectivities');
#19997=UNCERTAINTY_MEASURE_WITH_UNIT(LENGTH_MEASURE(0.001),#20097,
'DISTANCE_ACCURACY_VALUE',
'Maximum model space distance between geometric entities at asserted c
onnectivities');
#19998=UNCERTAINTY_MEASURE_WITH_UNIT(LENGTH_MEASURE(0.001),#20097,
'DISTANCE_ACCURACY_VALUE',
'Maximum model space distance between geometric entities at asserted c
onnectivities');
#19999=UNCERTAINTY_MEASURE_WITH_UNIT(LENGTH_MEASURE(0.001),#20097,
'DISTANCE_ACCURACY_VALUE',
'Maximum model space distance between geometric entities at asserted c
onnectivities');
#20000=UNCERTAINTY_MEASURE_WITH_UNIT(LENGTH_MEASURE(0.001),#20097,
'DISTANCE_ACCURACY_VALUE',
'Maximum model space distance between geometric entities at asserted c
onnectivities');
#20001=UNCERTAINTY_MEASURE_WITH_UNIT(LENGTH_MEASURE(0.001),#20097,
'DISTANCE_ACCURACY_VALUE',
'Maximum model space distance between geometric entities at asserted c
onnectivities');
#20002=UNCERTAINTY_MEASURE_WITH_UNIT(LENGTH_MEASURE(0.001),#20097,
'DISTANCE_ACCURACY_VALUE',
'Maximum model space distance between geometric entities at asserted c
onnectivities');
#20003=UNCERTAINTY_MEASURE_WITH_UNIT(LENGTH_MEASURE(0.001),#20097,
'DISTANCE_ACCURACY_VALUE',
'Maximum model space distance between geometric entities at asserted c
onnectivities');
#20004=UNCERTAINTY_MEASURE_WITH_UNIT(LENGTH_MEASURE(0.001),#20097,
'DISTANCE_ACCURACY_VALUE',
'Maximum model space distance between geometric entities at asserted c
onnectivities');
#20005=UNCERTAINTY_MEASURE_WITH_UNIT(LENGTH_MEASURE(0.001),#20097,
'DISTANCE_ACCURACY_VALUE',
'Maximum model space distance between geometric entities at asserted c
onnectivities');
#20006=UNCERTAINTY_MEASURE_WITH_UNIT(LENGTH_MEASURE(0.001),#20097,
'DISTANCE_ACCURACY_VALUE',
'Maximum model space distance between geometric entities at asserted c
onnectivities');
#20007=UNCERTAINTY_MEASURE_WITH_UNIT(LENGTH_MEASURE(0.001),#20097,
'DISTANCE_ACCURACY_VALUE',
'Maximum model space distance between geometric entities at asserted c
onnectivities');
#20008=UNCERTAINTY_MEASURE_WITH_UNIT(LENGTH_MEASURE(0.001),#20097,
'DISTANCE_ACCURACY_VALUE',
'Maximum model space distance between geometric entities at asserted c
onnectivities');
#20009=UNCERTAINTY_MEASURE_WITH_UNIT(LENGTH_MEASURE(0.001),#20097,
'DISTANCE_ACCURACY_VALUE',
'Maximum model space distance between geometric entities at asserted c
onnectivities');
#20010=UNCERTAINTY_MEASURE_WITH_UNIT(LENGTH_MEASURE(0.001),#20097,
'DISTANCE_ACCURACY_VALUE',
'Maximum model space distance between geometric entities at asserted c
onnectivities');
#20011=UNCERTAINTY_MEASURE_WITH_UNIT(LENGTH_MEASURE(0.001),#20097,
'DISTANCE_ACCURACY_VALUE',
'Maximum model space distance between geometric entities at asserted c
onnectivities');
#20012=UNCERTAINTY_MEASURE_WITH_UNIT(LENGTH_MEASURE(0.001),#20097,
'DISTANCE_ACCURACY_VALUE',
'Maximum model space distance between geometric entities at asserted c
onnectivities');
#20013=UNCERTAINTY_MEASURE_WITH_UNIT(LENGTH_MEASURE(0.001),#20097,
'DISTANCE_ACCURACY_VALUE',
'Maximum model space distance between geometric entities at asserted c
onnectivities');
#20014=UNCERTAINTY_MEASURE_WITH_UNIT(LENGTH_MEASURE(0.001),#20097,
'DISTANCE_ACCURACY_VALUE',
'Maximum model space distance between geometric entities at asserted c
onnectivities');
#20015=UNCERTAINTY_MEASURE_WITH_UNIT(LENGTH_MEASURE(0.001),#20097,
'DISTANCE_ACCURACY_VALUE',
'Maximum model space distance between geometric entities at asserted c
onnectivities');
#20016=UNCERTAINTY_MEASURE_WITH_UNIT(LENGTH_MEASURE(0.001),#20097,
'DISTANCE_ACCURACY_VALUE',
'Maximum model space distance between geometric entities at asserted c
onnectivities');
#20017=UNCERTAINTY_MEASURE_WITH_UNIT(LENGTH_MEASURE(0.001),#20097,
'DISTANCE_ACCURACY_VALUE',
'Maximum model space distance between geometric entities at asserted c
onnectivities');
#20018=UNCERTAINTY_MEASURE_WITH_UNIT(LENGTH_MEASURE(0.001),#20097,
'DISTANCE_ACCURACY_VALUE',
'Maximum model space distance between geometric entities at asserted c
onnectivities');
#20019=UNCERTAINTY_MEASURE_WITH_UNIT(LENGTH_MEASURE(0.001),#20097,
'DISTANCE_ACCURACY_VALUE',
'Maximum model space distance between geometric entities at asserted c
onnectivities');
#20020=UNCERTAINTY_MEASURE_WITH_UNIT(LENGTH_MEASURE(0.001),#20097,
'DISTANCE_ACCURACY_VALUE',
'Maximum model space distance between geometric entities at asserted c
onnectivities');
#20021=UNCERTAINTY_MEASURE_WITH_UNIT(LENGTH_MEASURE(0.001),#20097,
'DISTANCE_ACCURACY_VALUE',
'Maximum model space distance between geometric entities at asserted c
onnectivities');
#20022=UNCERTAINTY_MEASURE_WITH_UNIT(LENGTH_MEASURE(0.001),#20097,
'DISTANCE_ACCURACY_VALUE',
'Maximum model space distance between geometric entities at asserted c
onnectivities');
#20023=UNCERTAINTY_MEASURE_WITH_UNIT(LENGTH_MEASURE(0.001),#20097,
'DISTANCE_ACCURACY_VALUE',
'Maximum model space distance between geometric entities at asserted c
onnectivities');
#20024=UNCERTAINTY_MEASURE_WITH_UNIT(LENGTH_MEASURE(0.001),#20097,
'DISTANCE_ACCURACY_VALUE',
'Maximum model space distance between geometric entities at asserted c
onnectivities');
#20025=UNCERTAINTY_MEASURE_WITH_UNIT(LENGTH_MEASURE(0.001),#20097,
'DISTANCE_ACCURACY_VALUE',
'Maximum model space distance between geometric entities at asserted c
onnectivities');
#20026=UNCERTAINTY_MEASURE_WITH_UNIT(LENGTH_MEASURE(0.001),#20097,
'DISTANCE_ACCURACY_VALUE',
'Maximum model space distance between geometric entities at asserted c
onnectivities');
#20027=UNCERTAINTY_MEASURE_WITH_UNIT(LENGTH_MEASURE(0.001),#20097,
'DISTANCE_ACCURACY_VALUE',
'Maximum model space distance between geometric entities at asserted c
onnectivities');
#20028=UNCERTAINTY_MEASURE_WITH_UNIT(LENGTH_MEASURE(0.001),#20097,
'DISTANCE_ACCURACY_VALUE',
'Maximum model space distance between geometric entities at asserted c
onnectivities');
#20029=UNCERTAINTY_MEASURE_WITH_UNIT(LENGTH_MEASURE(0.001),#20097,
'DISTANCE_ACCURACY_VALUE',
'Maximum model space distance between geometric entities at asserted c
onnectivities');
#20030=UNCERTAINTY_MEASURE_WITH_UNIT(LENGTH_MEASURE(0.001),#20097,
'DISTANCE_ACCURACY_VALUE',
'Maximum model space distance between geometric entities at asserted c
onnectivities');
#20031=UNCERTAINTY_MEASURE_WITH_UNIT(LENGTH_MEASURE(0.001),#20097,
'DISTANCE_ACCURACY_VALUE',
'Maximum model space distance between geometric entities at asserted c
onnectivities');
#20032=UNCERTAINTY_MEASURE_WITH_UNIT(LENGTH_MEASURE(0.001),#20097,
'DISTANCE_ACCURACY_VALUE',
'Maximum model space distance between geometric entities at asserted c
onnectivities');
#20033=UNCERTAINTY_MEASURE_WITH_UNIT(LENGTH_MEASURE(0.001),#20097,
'DISTANCE_ACCURACY_VALUE',
'Maximum model space distance between geometric entities at asserted c
onnectivities');
#20034=UNCERTAINTY_MEASURE_WITH_UNIT(LENGTH_MEASURE(0.001),#20097,
'DISTANCE_ACCURACY_VALUE',
'Maximum model space distance between geometric entities at asserted c
onnectivities');
#20035=UNCERTAINTY_MEASURE_WITH_UNIT(LENGTH_MEASURE(0.001),#20097,
'DISTANCE_ACCURACY_VALUE',
'Maximum model space distance between geometric entities at asserted c
onnectivities');
#20036=UNCERTAINTY_MEASURE_WITH_UNIT(LENGTH_MEASURE(0.001),#20097,
'DISTANCE_ACCURACY_VALUE',
'Maximum model space distance between geometric entities at asserted c
onnectivities');
#20037=UNCERTAINTY_MEASURE_WITH_UNIT(LENGTH_MEASURE(0.001),#20097,
'DISTANCE_ACCURACY_VALUE',
'Maximum model space distance between geometric entities at asserted c
onnectivities');
#20038=UNCERTAINTY_MEASURE_WITH_UNIT(LENGTH_MEASURE(0.001),#20097,
'DISTANCE_ACCURACY_VALUE',
'Maximum model space distance between geometric entities at asserted c
onnectivities');
#20039=UNCERTAINTY_MEASURE_WITH_UNIT(LENGTH_MEASURE(0.001),#20097,
'DISTANCE_ACCURACY_VALUE',
'Maximum model space distance between geometric entities at asserted c
onnectivities');
#20040=UNCERTAINTY_MEASURE_WITH_UNIT(LENGTH_MEASURE(0.001),#20097,
'DISTANCE_ACCURACY_VALUE',
'Maximum model space distance between geometric entities at asserted c
onnectivities');
#20041=UNCERTAINTY_MEASURE_WITH_UNIT(LENGTH_MEASURE(0.001),#20097,
'DISTANCE_ACCURACY_VALUE',
'Maximum model space distance between geometric entities at asserted c
onnectivities');
#20042=UNCERTAINTY_MEASURE_WITH_UNIT(LENGTH_MEASURE(0.001),#20097,
'DISTANCE_ACCURACY_VALUE',
'Maximum model space distance between geometric entities at asserted c
onnectivities');
#20043=(
GEOMETRIC_REPRESENTATION_CONTEXT(3)
GLOBAL_UNCERTAINTY_ASSIGNED_CONTEXT((#19989))
GLOBAL_UNIT_ASSIGNED_CONTEXT((#20097,#20099,#20100))
REPRESENTATION_CONTEXT('','3D')
);
#20044=(
GEOMETRIC_REPRESENTATION_CONTEXT(3)
GLOBAL_UNCERTAINTY_ASSIGNED_CONTEXT((#19990))
GLOBAL_UNIT_ASSIGNED_CONTEXT((#20097,#20099,#20100))
REPRESENTATION_CONTEXT('','3D')
);
#20045=(
GEOMETRIC_REPRESENTATION_CONTEXT(3)
GLOBAL_UNCERTAINTY_ASSIGNED_CONTEXT((#19991))
GLOBAL_UNIT_ASSIGNED_CONTEXT((#20097,#20099,#20100))
REPRESENTATION_CONTEXT('','3D')
);
#20046=(
GEOMETRIC_REPRESENTATION_CONTEXT(3)
GLOBAL_UNCERTAINTY_ASSIGNED_CONTEXT((#19992))
GLOBAL_UNIT_ASSIGNED_CONTEXT((#20097,#20099,#20100))
REPRESENTATION_CONTEXT('','3D')
);
#20047=(
GEOMETRIC_REPRESENTATION_CONTEXT(3)
GLOBAL_UNCERTAINTY_ASSIGNED_CONTEXT((#19993))
GLOBAL_UNIT_ASSIGNED_CONTEXT((#20097,#20099,#20100))
REPRESENTATION_CONTEXT('','3D')
);
#20048=(
GEOMETRIC_REPRESENTATION_CONTEXT(3)
GLOBAL_UNCERTAINTY_ASSIGNED_CONTEXT((#19994))
GLOBAL_UNIT_ASSIGNED_CONTEXT((#20097,#20099,#20100))
REPRESENTATION_CONTEXT('','3D')
);
#20049=(
GEOMETRIC_REPRESENTATION_CONTEXT(3)
GLOBAL_UNCERTAINTY_ASSIGNED_CONTEXT((#19995))
GLOBAL_UNIT_ASSIGNED_CONTEXT((#20097,#20099,#20100))
REPRESENTATION_CONTEXT('','3D')
);
#20050=(
GEOMETRIC_REPRESENTATION_CONTEXT(3)
GLOBAL_UNCERTAINTY_ASSIGNED_CONTEXT((#19996))
GLOBAL_UNIT_ASSIGNED_CONTEXT((#20097,#20099,#20100))
REPRESENTATION_CONTEXT('','3D')
);
#20051=(
GEOMETRIC_REPRESENTATION_CONTEXT(3)
GLOBAL_UNCERTAINTY_ASSIGNED_CONTEXT((#19997))
GLOBAL_UNIT_ASSIGNED_CONTEXT((#20097,#20099,#20100))
REPRESENTATION_CONTEXT('','3D')
);
#20052=(
GEOMETRIC_REPRESENTATION_CONTEXT(3)
GLOBAL_UNCERTAINTY_ASSIGNED_CONTEXT((#19998))
GLOBAL_UNIT_ASSIGNED_CONTEXT((#20097,#20099,#20100))
REPRESENTATION_CONTEXT('','3D')
);
#20053=(
GEOMETRIC_REPRESENTATION_CONTEXT(3)
GLOBAL_UNCERTAINTY_ASSIGNED_CONTEXT((#19999))
GLOBAL_UNIT_ASSIGNED_CONTEXT((#20097,#20099,#20100))
REPRESENTATION_CONTEXT('','3D')
);
#20054=(
GEOMETRIC_REPRESENTATION_CONTEXT(3)
GLOBAL_UNCERTAINTY_ASSIGNED_CONTEXT((#20000))
GLOBAL_UNIT_ASSIGNED_CONTEXT((#20097,#20099,#20100))
REPRESENTATION_CONTEXT('','3D')
);
#20055=(
GEOMETRIC_REPRESENTATION_CONTEXT(3)
GLOBAL_UNCERTAINTY_ASSIGNED_CONTEXT((#20001))
GLOBAL_UNIT_ASSIGNED_CONTEXT((#20097,#20099,#20100))
REPRESENTATION_CONTEXT('','3D')
);
#20056=(
GEOMETRIC_REPRESENTATION_CONTEXT(3)
GLOBAL_UNCERTAINTY_ASSIGNED_CONTEXT((#20002))
GLOBAL_UNIT_ASSIGNED_CONTEXT((#20097,#20099,#20100))
REPRESENTATION_CONTEXT('','3D')
);
#20057=(
GEOMETRIC_REPRESENTATION_CONTEXT(3)
GLOBAL_UNCERTAINTY_ASSIGNED_CONTEXT((#20003))
GLOBAL_UNIT_ASSIGNED_CONTEXT((#20097,#20099,#20100))
REPRESENTATION_CONTEXT('','3D')
);
#20058=(
GEOMETRIC_REPRESENTATION_CONTEXT(3)
GLOBAL_UNCERTAINTY_ASSIGNED_CONTEXT((#20004))
GLOBAL_UNIT_ASSIGNED_CONTEXT((#20097,#20099,#20100))
REPRESENTATION_CONTEXT('','3D')
);
#20059=(
GEOMETRIC_REPRESENTATION_CONTEXT(3)
GLOBAL_UNCERTAINTY_ASSIGNED_CONTEXT((#20005))
GLOBAL_UNIT_ASSIGNED_CONTEXT((#20097,#20099,#20100))
REPRESENTATION_CONTEXT('','3D')
);
#20060=(
GEOMETRIC_REPRESENTATION_CONTEXT(3)
GLOBAL_UNCERTAINTY_ASSIGNED_CONTEXT((#20006))
GLOBAL_UNIT_ASSIGNED_CONTEXT((#20097,#20099,#20100))
REPRESENTATION_CONTEXT('','3D')
);
#20061=(
GEOMETRIC_REPRESENTATION_CONTEXT(3)
GLOBAL_UNCERTAINTY_ASSIGNED_CONTEXT((#20007))
GLOBAL_UNIT_ASSIGNED_CONTEXT((#20097,#20099,#20100))
REPRESENTATION_CONTEXT('','3D')
);
#20062=(
GEOMETRIC_REPRESENTATION_CONTEXT(3)
GLOBAL_UNCERTAINTY_ASSIGNED_CONTEXT((#20008))
GLOBAL_UNIT_ASSIGNED_CONTEXT((#20097,#20099,#20100))
REPRESENTATION_CONTEXT('','3D')
);
#20063=(
GEOMETRIC_REPRESENTATION_CONTEXT(3)
GLOBAL_UNCERTAINTY_ASSIGNED_CONTEXT((#20009))
GLOBAL_UNIT_ASSIGNED_CONTEXT((#20097,#20099,#20100))
REPRESENTATION_CONTEXT('','3D')
);
#20064=(
GEOMETRIC_REPRESENTATION_CONTEXT(3)
GLOBAL_UNCERTAINTY_ASSIGNED_CONTEXT((#20010))
GLOBAL_UNIT_ASSIGNED_CONTEXT((#20097,#20099,#20100))
REPRESENTATION_CONTEXT('','3D')
);
#20065=(
GEOMETRIC_REPRESENTATION_CONTEXT(3)
GLOBAL_UNCERTAINTY_ASSIGNED_CONTEXT((#20011))
GLOBAL_UNIT_ASSIGNED_CONTEXT((#20097,#20099,#20100))
REPRESENTATION_CONTEXT('','3D')
);
#20066=(
GEOMETRIC_REPRESENTATION_CONTEXT(3)
GLOBAL_UNCERTAINTY_ASSIGNED_CONTEXT((#20012))
GLOBAL_UNIT_ASSIGNED_CONTEXT((#20097,#20099,#20100))
REPRESENTATION_CONTEXT('','3D')
);
#20067=(
GEOMETRIC_REPRESENTATION_CONTEXT(3)
GLOBAL_UNCERTAINTY_ASSIGNED_CONTEXT((#20013))
GLOBAL_UNIT_ASSIGNED_CONTEXT((#20097,#20099,#20100))
REPRESENTATION_CONTEXT('','3D')
);
#20068=(
GEOMETRIC_REPRESENTATION_CONTEXT(3)
GLOBAL_UNCERTAINTY_ASSIGNED_CONTEXT((#20014))
GLOBAL_UNIT_ASSIGNED_CONTEXT((#20097,#20099,#20100))
REPRESENTATION_CONTEXT('','3D')
);
#20069=(
GEOMETRIC_REPRESENTATION_CONTEXT(3)
GLOBAL_UNCERTAINTY_ASSIGNED_CONTEXT((#20015))
GLOBAL_UNIT_ASSIGNED_CONTEXT((#20097,#20099,#20100))
REPRESENTATION_CONTEXT('','3D')
);
#20070=(
GEOMETRIC_REPRESENTATION_CONTEXT(3)
GLOBAL_UNCERTAINTY_ASSIGNED_CONTEXT((#20016))
GLOBAL_UNIT_ASSIGNED_CONTEXT((#20097,#20099,#20100))
REPRESENTATION_CONTEXT('','3D')
);
#20071=(
GEOMETRIC_REPRESENTATION_CONTEXT(3)
GLOBAL_UNCERTAINTY_ASSIGNED_CONTEXT((#20017))
GLOBAL_UNIT_ASSIGNED_CONTEXT((#20097,#20099,#20100))
REPRESENTATION_CONTEXT('','3D')
);
#20072=(
GEOMETRIC_REPRESENTATION_CONTEXT(3)
GLOBAL_UNCERTAINTY_ASSIGNED_CONTEXT((#20018))
GLOBAL_UNIT_ASSIGNED_CONTEXT((#20097,#20099,#20100))
REPRESENTATION_CONTEXT('','3D')
);
#20073=(
GEOMETRIC_REPRESENTATION_CONTEXT(3)
GLOBAL_UNCERTAINTY_ASSIGNED_CONTEXT((#20019))
GLOBAL_UNIT_ASSIGNED_CONTEXT((#20097,#20099,#20100))
REPRESENTATION_CONTEXT('','3D')
);
#20074=(
GEOMETRIC_REPRESENTATION_CONTEXT(3)
GLOBAL_UNCERTAINTY_ASSIGNED_CONTEXT((#20020))
GLOBAL_UNIT_ASSIGNED_CONTEXT((#20097,#20099,#20100))
REPRESENTATION_CONTEXT('','3D')
);
#20075=(
GEOMETRIC_REPRESENTATION_CONTEXT(3)
GLOBAL_UNCERTAINTY_ASSIGNED_CONTEXT((#20021))
GLOBAL_UNIT_ASSIGNED_CONTEXT((#20097,#20099,#20100))
REPRESENTATION_CONTEXT('','3D')
);
#20076=(
GEOMETRIC_REPRESENTATION_CONTEXT(3)
GLOBAL_UNCERTAINTY_ASSIGNED_CONTEXT((#20022))
GLOBAL_UNIT_ASSIGNED_CONTEXT((#20097,#20099,#20100))
REPRESENTATION_CONTEXT('','3D')
);
#20077=(
GEOMETRIC_REPRESENTATION_CONTEXT(3)
GLOBAL_UNCERTAINTY_ASSIGNED_CONTEXT((#20023))
GLOBAL_UNIT_ASSIGNED_CONTEXT((#20097,#20099,#20100))
REPRESENTATION_CONTEXT('','3D')
);
#20078=(
GEOMETRIC_REPRESENTATION_CONTEXT(3)
GLOBAL_UNCERTAINTY_ASSIGNED_CONTEXT((#20024))
GLOBAL_UNIT_ASSIGNED_CONTEXT((#20097,#20099,#20100))
REPRESENTATION_CONTEXT('','3D')
);
#20079=(
GEOMETRIC_REPRESENTATION_CONTEXT(3)
GLOBAL_UNCERTAINTY_ASSIGNED_CONTEXT((#20025))
GLOBAL_UNIT_ASSIGNED_CONTEXT((#20097,#20099,#20100))
REPRESENTATION_CONTEXT('','3D')
);
#20080=(
GEOMETRIC_REPRESENTATION_CONTEXT(3)
GLOBAL_UNCERTAINTY_ASSIGNED_CONTEXT((#20026))
GLOBAL_UNIT_ASSIGNED_CONTEXT((#20097,#20099,#20100))
REPRESENTATION_CONTEXT('','3D')
);
#20081=(
GEOMETRIC_REPRESENTATION_CONTEXT(3)
GLOBAL_UNCERTAINTY_ASSIGNED_CONTEXT((#20027))
GLOBAL_UNIT_ASSIGNED_CONTEXT((#20097,#20099,#20100))
REPRESENTATION_CONTEXT('','3D')
);
#20082=(
GEOMETRIC_REPRESENTATION_CONTEXT(3)
GLOBAL_UNCERTAINTY_ASSIGNED_CONTEXT((#20028))
GLOBAL_UNIT_ASSIGNED_CONTEXT((#20097,#20099,#20100))
REPRESENTATION_CONTEXT('','3D')
);
#20083=(
GEOMETRIC_REPRESENTATION_CONTEXT(3)
GLOBAL_UNCERTAINTY_ASSIGNED_CONTEXT((#20029))
GLOBAL_UNIT_ASSIGNED_CONTEXT((#20097,#20099,#20100))
REPRESENTATION_CONTEXT('','3D')
);
#20084=(
GEOMETRIC_REPRESENTATION_CONTEXT(3)
GLOBAL_UNCERTAINTY_ASSIGNED_CONTEXT((#20030))
GLOBAL_UNIT_ASSIGNED_CONTEXT((#20097,#20099,#20100))
REPRESENTATION_CONTEXT('','3D')
);
#20085=(
GEOMETRIC_REPRESENTATION_CONTEXT(3)
GLOBAL_UNCERTAINTY_ASSIGNED_CONTEXT((#20031))
GLOBAL_UNIT_ASSIGNED_CONTEXT((#20097,#20099,#20100))
REPRESENTATION_CONTEXT('','3D')
);
#20086=(
GEOMETRIC_REPRESENTATION_CONTEXT(3)
GLOBAL_UNCERTAINTY_ASSIGNED_CONTEXT((#20032))
GLOBAL_UNIT_ASSIGNED_CONTEXT((#20097,#20099,#20100))
REPRESENTATION_CONTEXT('','3D')
);
#20087=(
GEOMETRIC_REPRESENTATION_CONTEXT(3)
GLOBAL_UNCERTAINTY_ASSIGNED_CONTEXT((#20033))
GLOBAL_UNIT_ASSIGNED_CONTEXT((#20097,#20099,#20100))
REPRESENTATION_CONTEXT('','3D')
);
#20088=(
GEOMETRIC_REPRESENTATION_CONTEXT(3)
GLOBAL_UNCERTAINTY_ASSIGNED_CONTEXT((#20034))
GLOBAL_UNIT_ASSIGNED_CONTEXT((#20097,#20099,#20100))
REPRESENTATION_CONTEXT('','3D')
);
#20089=(
GEOMETRIC_REPRESENTATION_CONTEXT(3)
GLOBAL_UNCERTAINTY_ASSIGNED_CONTEXT((#20035))
GLOBAL_UNIT_ASSIGNED_CONTEXT((#20097,#20099,#20100))
REPRESENTATION_CONTEXT('','3D')
);
#20090=(
GEOMETRIC_REPRESENTATION_CONTEXT(3)
GLOBAL_UNCERTAINTY_ASSIGNED_CONTEXT((#20036))
GLOBAL_UNIT_ASSIGNED_CONTEXT((#20097,#20099,#20100))
REPRESENTATION_CONTEXT('','3D')
);
#20091=(
GEOMETRIC_REPRESENTATION_CONTEXT(3)
GLOBAL_UNCERTAINTY_ASSIGNED_CONTEXT((#20037))
GLOBAL_UNIT_ASSIGNED_CONTEXT((#20097,#20099,#20100))
REPRESENTATION_CONTEXT('','3D')
);
#20092=(
GEOMETRIC_REPRESENTATION_CONTEXT(3)
GLOBAL_UNCERTAINTY_ASSIGNED_CONTEXT((#20038))
GLOBAL_UNIT_ASSIGNED_CONTEXT((#20097,#20099,#20100))
REPRESENTATION_CONTEXT('','3D')
);
#20093=(
GEOMETRIC_REPRESENTATION_CONTEXT(3)
GLOBAL_UNCERTAINTY_ASSIGNED_CONTEXT((#20039))
GLOBAL_UNIT_ASSIGNED_CONTEXT((#20097,#20099,#20100))
REPRESENTATION_CONTEXT('','3D')
);
#20094=(
GEOMETRIC_REPRESENTATION_CONTEXT(3)
GLOBAL_UNCERTAINTY_ASSIGNED_CONTEXT((#20040))
GLOBAL_UNIT_ASSIGNED_CONTEXT((#20097,#20099,#20100))
REPRESENTATION_CONTEXT('','3D')
);
#20095=(
GEOMETRIC_REPRESENTATION_CONTEXT(3)
GLOBAL_UNCERTAINTY_ASSIGNED_CONTEXT((#20041))
GLOBAL_UNIT_ASSIGNED_CONTEXT((#20097,#20099,#20100))
REPRESENTATION_CONTEXT('','3D')
);
#20096=(
GEOMETRIC_REPRESENTATION_CONTEXT(3)
GLOBAL_UNCERTAINTY_ASSIGNED_CONTEXT((#20042))
GLOBAL_UNIT_ASSIGNED_CONTEXT((#20097,#20099,#20100))
REPRESENTATION_CONTEXT('','3D')
);
#20097=(
LENGTH_UNIT()
NAMED_UNIT(*)
SI_UNIT(.CENTI.,.METRE.)
);
#20098=(
LENGTH_UNIT()
NAMED_UNIT(*)
SI_UNIT($,.METRE.)
);
#20099=(
NAMED_UNIT(*)
PLANE_ANGLE_UNIT()
SI_UNIT($,.RADIAN.)
);
#20100=(
NAMED_UNIT(*)
SI_UNIT($,.STERADIAN.)
SOLID_ANGLE_UNIT()
);
#20101=SHAPE_DEFINITION_REPRESENTATION(#20154,#20312);
#20102=SHAPE_DEFINITION_REPRESENTATION(#20155,#20313);
#20103=SHAPE_DEFINITION_REPRESENTATION(#20156,#20314);
#20104=SHAPE_DEFINITION_REPRESENTATION(#20157,#20315);
#20105=SHAPE_DEFINITION_REPRESENTATION(#20158,#20316);
#20106=SHAPE_DEFINITION_REPRESENTATION(#20159,#20317);
#20107=SHAPE_DEFINITION_REPRESENTATION(#20160,#20318);
#20108=SHAPE_DEFINITION_REPRESENTATION(#20161,#20319);
#20109=SHAPE_DEFINITION_REPRESENTATION(#20162,#20320);
#20110=SHAPE_DEFINITION_REPRESENTATION(#20163,#20321);
#20111=SHAPE_DEFINITION_REPRESENTATION(#20164,#20322);
#20112=SHAPE_DEFINITION_REPRESENTATION(#20165,#20323);
#20113=SHAPE_DEFINITION_REPRESENTATION(#20166,#20324);
#20114=SHAPE_DEFINITION_REPRESENTATION(#20167,#20325);
#20115=SHAPE_DEFINITION_REPRESENTATION(#20168,#20326);
#20116=SHAPE_DEFINITION_REPRESENTATION(#20169,#20327);
#20117=SHAPE_DEFINITION_REPRESENTATION(#20170,#20328);
#20118=SHAPE_DEFINITION_REPRESENTATION(#20171,#20329);
#20119=SHAPE_DEFINITION_REPRESENTATION(#20172,#20330);
#20120=SHAPE_DEFINITION_REPRESENTATION(#20173,#20331);
#20121=SHAPE_DEFINITION_REPRESENTATION(#20174,#20332);
#20122=SHAPE_DEFINITION_REPRESENTATION(#20175,#20333);
#20123=SHAPE_DEFINITION_REPRESENTATION(#20181,#20334);
#20124=SHAPE_DEFINITION_REPRESENTATION(#20182,#20335);
#20125=SHAPE_DEFINITION_REPRESENTATION(#20183,#20336);
#20126=SHAPE_DEFINITION_REPRESENTATION(#20184,#20337);
#20127=SHAPE_DEFINITION_REPRESENTATION(#20185,#20338);
#20128=SHAPE_DEFINITION_REPRESENTATION(#20186,#20339);
#20129=SHAPE_DEFINITION_REPRESENTATION(#20187,#20340);
#20130=SHAPE_DEFINITION_REPRESENTATION(#20188,#20341);
#20131=SHAPE_DEFINITION_REPRESENTATION(#20189,#20342);
#20132=SHAPE_DEFINITION_REPRESENTATION(#20190,#20343);
#20133=SHAPE_DEFINITION_REPRESENTATION(#20191,#20344);
#20134=SHAPE_DEFINITION_REPRESENTATION(#20192,#20345);
#20135=SHAPE_DEFINITION_REPRESENTATION(#20193,#20346);
#20136=SHAPE_DEFINITION_REPRESENTATION(#20194,#20347);
#20137=SHAPE_DEFINITION_REPRESENTATION(#20195,#20348);
#20138=SHAPE_DEFINITION_REPRESENTATION(#20196,#20349);
#20139=SHAPE_DEFINITION_REPRESENTATION(#20197,#20350);
#20140=SHAPE_DEFINITION_REPRESENTATION(#20198,#20351);
#20141=SHAPE_DEFINITION_REPRESENTATION(#20199,#20352);
#20142=SHAPE_DEFINITION_REPRESENTATION(#20200,#20353);
#20143=SHAPE_DEFINITION_REPRESENTATION(#20201,#20354);
#20144=SHAPE_DEFINITION_REPRESENTATION(#20202,#20355);
#20145=SHAPE_DEFINITION_REPRESENTATION(#20203,#20356);
#20146=SHAPE_DEFINITION_REPRESENTATION(#20204,#20357);
#20147=SHAPE_DEFINITION_REPRESENTATION(#20205,#20358);
#20148=SHAPE_DEFINITION_REPRESENTATION(#20206,#20359);
#20149=SHAPE_DEFINITION_REPRESENTATION(#20207,#20360);
#20150=SHAPE_DEFINITION_REPRESENTATION(#20211,#20361);
#20151=SHAPE_DEFINITION_REPRESENTATION(#20212,#20362);
#20152=SHAPE_DEFINITION_REPRESENTATION(#20213,#20363);
#20153=SHAPE_DEFINITION_REPRESENTATION(#20214,#20364);
#20154=PRODUCT_DEFINITION_SHAPE('',$,#20366);
#20155=PRODUCT_DEFINITION_SHAPE('',$,#20367);
#20156=PRODUCT_DEFINITION_SHAPE('',$,#20368);
#20157=PRODUCT_DEFINITION_SHAPE('',$,#20369);
#20158=PRODUCT_DEFINITION_SHAPE('',$,#20370);
#20159=PRODUCT_DEFINITION_SHAPE('',$,#20371);
#20160=PRODUCT_DEFINITION_SHAPE('',$,#20372);
#20161=PRODUCT_DEFINITION_SHAPE('',$,#20373);
#20162=PRODUCT_DEFINITION_SHAPE('',$,#20374);
#20163=PRODUCT_DEFINITION_SHAPE('',$,#20375);
#20164=PRODUCT_DEFINITION_SHAPE('',$,#20376);
#20165=PRODUCT_DEFINITION_SHAPE('',$,#20377);
#20166=PRODUCT_DEFINITION_SHAPE('',$,#20378);
#20167=PRODUCT_DEFINITION_SHAPE('',$,#20379);
#20168=PRODUCT_DEFINITION_SHAPE('',$,#20380);
#20169=PRODUCT_DEFINITION_SHAPE('',$,#20381);
#20170=PRODUCT_DEFINITION_SHAPE('',$,#20382);
#20171=PRODUCT_DEFINITION_SHAPE('',$,#20383);
#20172=PRODUCT_DEFINITION_SHAPE('',$,#20384);
#20173=PRODUCT_DEFINITION_SHAPE('',$,#20385);
#20174=PRODUCT_DEFINITION_SHAPE('',$,#20386);
#20175=PRODUCT_DEFINITION_SHAPE('',$,#20387);
#20176=PRODUCT_DEFINITION_SHAPE($,$,#336);
#20177=PRODUCT_DEFINITION_SHAPE($,$,#337);
#20178=PRODUCT_DEFINITION_SHAPE($,$,#338);
#20179=PRODUCT_DEFINITION_SHAPE($,$,#339);
#20180=PRODUCT_DEFINITION_SHAPE($,$,#340);
#20181=PRODUCT_DEFINITION_SHAPE('',$,#20388);
#20182=PRODUCT_DEFINITION_SHAPE('',$,#20389);
#20183=PRODUCT_DEFINITION_SHAPE('',$,#20390);
#20184=PRODUCT_DEFINITION_SHAPE('',$,#20391);
#20185=PRODUCT_DEFINITION_SHAPE('',$,#20392);
#20186=PRODUCT_DEFINITION_SHAPE('',$,#20393);
#20187=PRODUCT_DEFINITION_SHAPE('',$,#20394);
#20188=PRODUCT_DEFINITION_SHAPE('',$,#20395);
#20189=PRODUCT_DEFINITION_SHAPE('',$,#20396);
#20190=PRODUCT_DEFINITION_SHAPE('',$,#20397);
#20191=PRODUCT_DEFINITION_SHAPE('',$,#20398);
#20192=PRODUCT_DEFINITION_SHAPE('',$,#20399);
#20193=PRODUCT_DEFINITION_SHAPE('',$,#20400);
#20194=PRODUCT_DEFINITION_SHAPE('',$,#20401);
#20195=PRODUCT_DEFINITION_SHAPE('',$,#20402);
#20196=PRODUCT_DEFINITION_SHAPE('',$,#20403);
#20197=PRODUCT_DEFINITION_SHAPE('',$,#20404);
#20198=PRODUCT_DEFINITION_SHAPE('',$,#20405);
#20199=PRODUCT_DEFINITION_SHAPE('',$,#20406);
#20200=PRODUCT_DEFINITION_SHAPE('',$,#20407);
#20201=PRODUCT_DEFINITION_SHAPE('',$,#20408);
#20202=PRODUCT_DEFINITION_SHAPE('',$,#20409);
#20203=PRODUCT_DEFINITION_SHAPE('',$,#20410);
#20204=PRODUCT_DEFINITION_SHAPE('',$,#20411);
#20205=PRODUCT_DEFINITION_SHAPE('',$,#20412);
#20206=PRODUCT_DEFINITION_SHAPE('',$,#20413);
#20207=PRODUCT_DEFINITION_SHAPE('',$,#20414);
#20208=PRODUCT_DEFINITION_SHAPE($,$,#341);
#20209=PRODUCT_DEFINITION_SHAPE($,$,#342);
#20210=PRODUCT_DEFINITION_SHAPE($,$,#343);
#20211=PRODUCT_DEFINITION_SHAPE('',$,#20415);
#20212=PRODUCT_DEFINITION_SHAPE('',$,#20416);
#20213=PRODUCT_DEFINITION_SHAPE('',$,#20417);
#20214=PRODUCT_DEFINITION_SHAPE('',$,#20418);
#20215=PRODUCT_DEFINITION_SHAPE($,$,#344);
#20216=PRODUCT_DEFINITION_SHAPE($,$,#345);
#20217=PRODUCT_DEFINITION_SHAPE($,$,#346);
#20218=PRODUCT_DEFINITION_SHAPE($,$,#347);
#20219=PRODUCT_DEFINITION_SHAPE($,$,#348);
#20220=PRODUCT_DEFINITION_SHAPE($,$,#349);
#20221=PRODUCT_DEFINITION_SHAPE($,$,#350);
#20222=PRODUCT_DEFINITION_SHAPE($,$,#351);
#20223=PRODUCT_DEFINITION_SHAPE($,$,#352);
#20224=PRODUCT_DEFINITION_SHAPE($,$,#353);
#20225=PRODUCT_DEFINITION_SHAPE($,$,#354);
#20226=PRODUCT_DEFINITION_SHAPE($,$,#355);
#20227=PRODUCT_DEFINITION_SHAPE($,$,#356);
#20228=PRODUCT_DEFINITION_SHAPE($,$,#357);
#20229=PRODUCT_DEFINITION_SHAPE($,$,#358);
#20230=PRODUCT_DEFINITION_SHAPE($,$,#359);
#20231=PRODUCT_DEFINITION_SHAPE($,$,#360);
#20232=PRODUCT_DEFINITION_SHAPE($,$,#361);
#20233=PRODUCT_DEFINITION_SHAPE($,$,#362);
#20234=PRODUCT_DEFINITION_SHAPE($,$,#363);
#20235=PRODUCT_DEFINITION_SHAPE($,$,#364);
#20236=PRODUCT_DEFINITION_SHAPE($,$,#365);
#20237=PRODUCT_DEFINITION_SHAPE($,$,#366);
#20238=PRODUCT_DEFINITION_SHAPE($,$,#367);
#20239=PRODUCT_DEFINITION_SHAPE($,$,#368);
#20240=PRODUCT_DEFINITION_SHAPE($,$,#369);
#20241=PRODUCT_DEFINITION_SHAPE($,$,#370);
#20242=PRODUCT_DEFINITION_SHAPE($,$,#371);
#20243=PRODUCT_DEFINITION_SHAPE($,$,#372);
#20244=PRODUCT_DEFINITION_SHAPE($,$,#373);
#20245=PRODUCT_DEFINITION_SHAPE($,$,#374);
#20246=PRODUCT_DEFINITION_SHAPE($,$,#375);
#20247=PRODUCT_DEFINITION_SHAPE($,$,#376);
#20248=PRODUCT_DEFINITION_SHAPE($,$,#377);
#20249=PRODUCT_DEFINITION_SHAPE($,$,#378);
#20250=PRODUCT_DEFINITION_SHAPE($,$,#379);
#20251=PRODUCT_DEFINITION_SHAPE($,$,#380);
#20252=PRODUCT_DEFINITION_SHAPE($,$,#381);
#20253=PRODUCT_DEFINITION_SHAPE($,$,#382);
#20254=PRODUCT_DEFINITION_SHAPE($,$,#383);
#20255=PRODUCT_DEFINITION_SHAPE($,$,#384);
#20256=PRODUCT_DEFINITION_SHAPE($,$,#385);
#20257=PRODUCT_DEFINITION_SHAPE($,$,#386);
#20258=PRODUCT_DEFINITION_SHAPE($,$,#387);
#20259=PRODUCT_DEFINITION_SHAPE($,$,#388);
#20260=PRODUCT_DEFINITION_SHAPE($,$,#389);
#20261=PRODUCT_DEFINITION_SHAPE($,$,#390);
#20262=PRODUCT_DEFINITION_SHAPE($,$,#391);
#20263=PRODUCT_DEFINITION_SHAPE($,$,#392);
#20264=PRODUCT_DEFINITION_SHAPE($,$,#393);
#20265=PRODUCT_DEFINITION_SHAPE($,$,#394);
#20266=PRODUCT_DEFINITION_SHAPE($,$,#395);
#20267=PRODUCT_DEFINITION_SHAPE($,$,#396);
#20268=PRODUCT_DEFINITION_SHAPE($,$,#397);
#20269=PRODUCT_DEFINITION_SHAPE($,$,#398);
#20270=PRODUCT_DEFINITION_SHAPE($,$,#399);
#20271=PRODUCT_DEFINITION_SHAPE($,$,#400);
#20272=PRODUCT_DEFINITION_SHAPE($,$,#401);
#20273=PRODUCT_DEFINITION_SHAPE($,$,#402);
#20274=PRODUCT_DEFINITION_SHAPE($,$,#403);
#20275=PRODUCT_DEFINITION_SHAPE($,$,#404);
#20276=PRODUCT_DEFINITION_SHAPE($,$,#405);
#20277=PRODUCT_DEFINITION_SHAPE($,$,#406);
#20278=PRODUCT_DEFINITION_SHAPE($,$,#407);
#20279=PRODUCT_DEFINITION_SHAPE($,$,#408);
#20280=PRODUCT_DEFINITION_SHAPE($,$,#409);
#20281=PRODUCT_DEFINITION_SHAPE($,$,#410);
#20282=PRODUCT_DEFINITION_SHAPE($,$,#411);
#20283=PRODUCT_DEFINITION_SHAPE($,$,#412);
#20284=PRODUCT_DEFINITION_SHAPE($,$,#413);
#20285=PRODUCT_DEFINITION_SHAPE($,$,#414);
#20286=PRODUCT_DEFINITION_SHAPE($,$,#415);
#20287=PRODUCT_DEFINITION_SHAPE($,$,#416);
#20288=PRODUCT_DEFINITION_SHAPE($,$,#417);
#20289=PRODUCT_DEFINITION_SHAPE($,$,#418);
#20290=PRODUCT_DEFINITION_SHAPE($,$,#419);
#20291=PRODUCT_DEFINITION_SHAPE($,$,#420);
#20292=PRODUCT_DEFINITION_SHAPE($,$,#421);
#20293=PRODUCT_DEFINITION_SHAPE($,$,#422);
#20294=PRODUCT_DEFINITION_SHAPE($,$,#423);
#20295=PRODUCT_DEFINITION_SHAPE($,$,#424);
#20296=PRODUCT_DEFINITION_SHAPE($,$,#425);
#20297=PRODUCT_DEFINITION_SHAPE($,$,#426);
#20298=PRODUCT_DEFINITION_SHAPE($,$,#427);
#20299=PRODUCT_DEFINITION_SHAPE($,$,#428);
#20300=PRODUCT_DEFINITION_SHAPE($,$,#429);
#20301=PRODUCT_DEFINITION_SHAPE($,$,#430);
#20302=PRODUCT_DEFINITION_SHAPE($,$,#431);
#20303=PRODUCT_DEFINITION_SHAPE($,$,#432);
#20304=PRODUCT_DEFINITION_SHAPE($,$,#433);
#20305=PRODUCT_DEFINITION_SHAPE($,$,#434);
#20306=PRODUCT_DEFINITION_SHAPE($,$,#435);
#20307=PRODUCT_DEFINITION_SHAPE($,$,#436);
#20308=PRODUCT_DEFINITION_SHAPE($,$,#437);
#20309=PRODUCT_DEFINITION_SHAPE($,$,#438);
#20310=PRODUCT_DEFINITION_SHAPE($,$,#439);
#20311=PRODUCT_DEFINITION_SHAPE($,$,#440);
#20312=SHAPE_REPRESENTATION('',(#11490,#12781,#12782,#12783,#12784),#20043);
#20313=SHAPE_REPRESENTATION('',(#11491,#12688,#12689,#12690,#12691,#12692,
#12693,#12694,#12695,#12696,#12697,#12698,#12699,#12700,#12701,#12702,#12703,
#12704,#12705,#12706,#12707,#12708,#12709,#12710,#12711,#12712,#12713,#12714,
#12715,#12716,#12717,#12718,#12719,#12720,#12721,#12722,#12723,#12724,#12725,
#12726,#12727,#12728,#12729,#12730,#12731,#12732,#12733,#12734,#12735,#12736,
#12737,#12738,#12739,#12740,#12741,#12742,#12743,#12744,#12745,#12746,#12747,
#12748),#20044);
#20314=SHAPE_REPRESENTATION('',(#11492),#20045);
#20315=SHAPE_REPRESENTATION('',(#11575),#20046);
#20316=SHAPE_REPRESENTATION('',(#11588),#20047);
#20317=SHAPE_REPRESENTATION('',(#11601),#20048);
#20318=SHAPE_REPRESENTATION('',(#11639),#20049);
#20319=SHAPE_REPRESENTATION('',(#11648),#20050);
#20320=SHAPE_REPRESENTATION('',(#11682),#20051);
#20321=SHAPE_REPRESENTATION('',(#11716),#20052);
#20322=SHAPE_REPRESENTATION('',(#11754),#20053);
#20323=SHAPE_REPRESENTATION('',(#11763),#20054);
#20324=SHAPE_REPRESENTATION('',(#11797),#20055);
#20325=SHAPE_REPRESENTATION('',(#11831),#20056);
#20326=SHAPE_REPRESENTATION('',(#11850),#20057);
#20327=SHAPE_REPRESENTATION('',(#11883),#20058);
#20328=SHAPE_REPRESENTATION('',(#11916,#12045,#12046,#12047,#12048,#12049),
#20059);
#20329=SHAPE_REPRESENTATION('',(#11917),#20060);
#20330=SHAPE_REPRESENTATION('',(#11937),#20061);
#20331=SHAPE_REPRESENTATION('',(#11957),#20062);
#20332=SHAPE_REPRESENTATION('',(#11974),#20063);
#20333=SHAPE_REPRESENTATION('',(#12028),#20064);
#20334=SHAPE_REPRESENTATION('',(#12050),#20065);
#20335=SHAPE_REPRESENTATION('',(#12100),#20066);
#20336=SHAPE_REPRESENTATION('',(#12121),#20067);
#20337=SHAPE_REPRESENTATION('',(#12145),#20068);
#20338=SHAPE_REPRESENTATION('',(#12188,#12749,#12750,#12751,#12752,#12753,
#12754,#12755,#12756),#20069);
#20339=SHAPE_REPRESENTATION('',(#12189),#20070);
#20340=SHAPE_REPRESENTATION('',(#12211),#20071);
#20341=SHAPE_REPRESENTATION('',(#12224),#20072);
#20342=SHAPE_REPRESENTATION('',(#12233),#20073);
#20343=SHAPE_REPRESENTATION('',(#12239),#20074);
#20344=SHAPE_REPRESENTATION('',(#12245),#20075);
#20345=SHAPE_REPRESENTATION('',(#12254,#12757,#12758,#12759,#12760,#12761,
#12762,#12763,#12764),#20076);
#20346=SHAPE_REPRESENTATION('',(#12255),#20077);
#20347=SHAPE_REPRESENTATION('',(#12277),#20078);
#20348=SHAPE_REPRESENTATION('',(#12290),#20079);
#20349=SHAPE_REPRESENTATION('',(#12299),#20080);
#20350=SHAPE_REPRESENTATION('',(#12305),#20081);
#20351=SHAPE_REPRESENTATION('',(#12311),#20082);
#20352=SHAPE_REPRESENTATION('',(#12320),#20083);
#20353=SHAPE_REPRESENTATION('',(#12462,#12765,#12766,#12767,#12768,#12769,
#12770,#12771,#12772,#12773,#12774,#12775,#12776,#12777,#12778,#12779,#12780),
#20084);
#20354=SHAPE_REPRESENTATION('',(#12463),#20085);
#20355=SHAPE_REPRESENTATION('',(#12496),#20086);
#20356=SHAPE_REPRESENTATION('',(#12529),#20087);
#20357=SHAPE_REPRESENTATION('',(#12536,#12598,#12599,#12600),#20088);
#20358=SHAPE_REPRESENTATION('',(#12537),#20089);
#20359=SHAPE_REPRESENTATION('',(#12576),#20090);
#20360=SHAPE_REPRESENTATION('',(#12587),#20091);
#20361=SHAPE_REPRESENTATION('',(#12601),#20092);
#20362=SHAPE_REPRESENTATION('',(#12612),#20093);
#20363=SHAPE_REPRESENTATION('',(#12638),#20094);
#20364=SHAPE_REPRESENTATION('',(#12662),#20095);
#20365=PRODUCT_DEFINITION_CONTEXT('part definition',#20526,'design');
#20366=PRODUCT_DEFINITION('PAT-013',
'PAT-013',#20419,#20365);
#20367=PRODUCT_DEFINITION('Frame and belt envelope',
'Frame and belt envelope',#20420,#20365);
#20368=PRODUCT_DEFINITION('Base','Base',#20421,#20365);
#20369=PRODUCT_DEFINITION('Foot','Foot',#20422,#20365);
#20370=PRODUCT_DEFINITION('Foot (1)','Foot (1)',#20423,#20365);
#20371=PRODUCT_DEFINITION('Fixed bearing block','Fixed bearing block',#20424,
#20365);
#20372=PRODUCT_DEFINITION('Input outer spacer','Input outer spacer',#20425,
#20365);
#20373=PRODUCT_DEFINITION('Input bearing cap','Input bearing cap',#20426,
#20365);
#20374=PRODUCT_DEFINITION('Input bearing cap (1)','Input bearing cap (1)',
#20427,#20365);
#20375=PRODUCT_DEFINITION('Fixed bearing block (1)',
'Fixed bearing block (1)',#20428,#20365);
#20376=PRODUCT_DEFINITION('Input outer spacer (1)',
'Input outer spacer (1)',#20429,#20365);
#20377=PRODUCT_DEFINITION('Input bearing cap (2)','Input bearing cap (2)',
#20430,#20365);
#20378=PRODUCT_DEFINITION('Input bearing cap (3)','Input bearing cap (3)',
#20431,#20365);
#20379=PRODUCT_DEFINITION('Timing belt backing envelope',
'Timing belt backing envelope',#20432,#20365);
#20380=PRODUCT_DEFINITION('Travel stop','Travel stop',#20433,#20365);
#20381=PRODUCT_DEFINITION('Travel stop (1)','Travel stop (1)',#20434,#20365);
#20382=PRODUCT_DEFINITION('Sealed Ball Bearing - 10 x 30 x 9 mm',
'Sealed Ball Bearing - 10 x 30 x 9 mm',#20435,#20365);
#20383=PRODUCT_DEFINITION('Inner ring','Inner ring',#20436,#20365);
#20384=PRODUCT_DEFINITION('Outer ring','Outer ring',#20437,#20365);
#20385=PRODUCT_DEFINITION('Balls','Balls',#20438,#20365);
#20386=PRODUCT_DEFINITION('Cage','Cage',#20439,#20365);
#20387=PRODUCT_DEFINITION('Seals 2RS','Seals 2RS',#20440,#20365);
#20388=PRODUCT_DEFINITION('Slotted Extrusion - 20 x 20 x 400 mm',
'Slotted Extrusion - 20 x 20 x 400 mm',#20441,#20365);
#20389=PRODUCT_DEFINITION('Captive slot nut','Captive slot nut',#20442,
#20365);
#20390=PRODUCT_DEFINITION('M5x17.5 extrusion screw',
'M5x17.5 extrusion screw',#20443,#20365);
#20391=PRODUCT_DEFINITION('Linear Guide Rail - 15 mm, 220 mm Long',
'Linear Guide Rail - 15 mm, 220 mm Long',#20444,#20365);
#20392=PRODUCT_DEFINITION('Drive pulley and shaft',
'Drive pulley and shaft',#20445,#20365);
#20393=PRODUCT_DEFINITION('Input shaft','Input shaft',#20446,#20365);
#20394=PRODUCT_DEFINITION('Input inner spacer','Input inner spacer',#20447,
#20365);
#20395=PRODUCT_DEFINITION('Input inner sleeve','Input inner sleeve',#20448,
#20365);
#20396=PRODUCT_DEFINITION('Input M3 set screw','Input M3 set screw',#20449,
#20365);
#20397=PRODUCT_DEFINITION('Input M3 set screw (1)',
'Input M3 set screw (1)',#20450,#20365);
#20398=PRODUCT_DEFINITION('Input end keeper','Input end keeper',#20451,
#20365);
#20399=PRODUCT_DEFINITION('Return pulley and shaft',
'Return pulley and shaft',#20452,#20365);
#20400=PRODUCT_DEFINITION('Input shaft (1)','Input shaft (1)',#20453,#20365);
#20401=PRODUCT_DEFINITION('Input inner spacer (1)',
'Input inner spacer (1)',#20454,#20365);
#20402=PRODUCT_DEFINITION('Input inner sleeve (1)',
'Input inner sleeve (1)',#20455,#20365);
#20403=PRODUCT_DEFINITION('Input M3 set screw (2)',
'Input M3 set screw (2)',#20456,#20365);
#20404=PRODUCT_DEFINITION('Input M3 set screw (3)',
'Input M3 set screw (3)',#20457,#20365);
#20405=PRODUCT_DEFINITION('Input end keeper (1)','Input end keeper (1)',#20458,
#20365);
#20406=PRODUCT_DEFINITION(
'Timing Pulley - 2 mm Pitch, 20 Teeth, 8 mm Bore',
'Timing Pulley - 2 mm Pitch, 20 Teeth, 8 mm Bore',#20459,#20365);
#20407=PRODUCT_DEFINITION('Moving carriage','Moving carriage',#20460,#20365);
#20408=PRODUCT_DEFINITION('Moving table','Moving table',#20461,#20365);
#20409=PRODUCT_DEFINITION('Belt attachment bracket',
'Belt attachment bracket',#20462,#20365);
#20410=PRODUCT_DEFINITION('Belt clamp jaw','Belt clamp jaw',#20463,#20365);
#20411=PRODUCT_DEFINITION('Flanged Linear Guide Carriage - 15 mm',
'Flanged Linear Guide Carriage - 15 mm',#20464,#20365);
#20412=PRODUCT_DEFINITION('Block','Block',#20465,#20365);
#20413=PRODUCT_DEFINITION('End cap +','End cap +',#20466,#20365);
#20414=PRODUCT_DEFINITION('End cap','End cap',#20467,#20365);
#20415=PRODUCT_DEFINITION('Flat Washer - M5','Flat Washer - M5',#20468,
#20365);
#20416=PRODUCT_DEFINITION('Cap Screw - M5x20','Cap Screw - M5x20',#20469,
#20365);
#20417=PRODUCT_DEFINITION('M4x10 Cap Screw','M4x10 Cap Screw',#20470,#20365);
#20418=PRODUCT_DEFINITION('Cap Screw - M4x16','Cap Screw - M4x16',#20471,
#20365);
#20419=PRODUCT_DEFINITION_FORMATION('',$,#20528);
#20420=PRODUCT_DEFINITION_FORMATION('',$,#20529);
#20421=PRODUCT_DEFINITION_FORMATION('',$,#20530);
#20422=PRODUCT_DEFINITION_FORMATION('',$,#20531);
#20423=PRODUCT_DEFINITION_FORMATION('',$,#20532);
#20424=PRODUCT_DEFINITION_FORMATION('',$,#20533);
#20425=PRODUCT_DEFINITION_FORMATION('',$,#20534);
#20426=PRODUCT_DEFINITION_FORMATION('',$,#20535);
#20427=PRODUCT_DEFINITION_FORMATION('',$,#20536);
#20428=PRODUCT_DEFINITION_FORMATION('',$,#20537);
#20429=PRODUCT_DEFINITION_FORMATION('',$,#20538);
#20430=PRODUCT_DEFINITION_FORMATION('',$,#20539);
#20431=PRODUCT_DEFINITION_FORMATION('',$,#20540);
#20432=PRODUCT_DEFINITION_FORMATION('',$,#20541);
#20433=PRODUCT_DEFINITION_FORMATION('',$,#20542);
#20434=PRODUCT_DEFINITION_FORMATION('',$,#20543);
#20435=PRODUCT_DEFINITION_FORMATION('',$,#20544);
#20436=PRODUCT_DEFINITION_FORMATION('',$,#20545);
#20437=PRODUCT_DEFINITION_FORMATION('',$,#20546);
#20438=PRODUCT_DEFINITION_FORMATION('',$,#20547);
#20439=PRODUCT_DEFINITION_FORMATION('',$,#20548);
#20440=PRODUCT_DEFINITION_FORMATION('',$,#20549);
#20441=PRODUCT_DEFINITION_FORMATION('',$,#20550);
#20442=PRODUCT_DEFINITION_FORMATION('',$,#20551);
#20443=PRODUCT_DEFINITION_FORMATION('',$,#20552);
#20444=PRODUCT_DEFINITION_FORMATION('',$,#20553);
#20445=PRODUCT_DEFINITION_FORMATION('',$,#20554);
#20446=PRODUCT_DEFINITION_FORMATION('',$,#20555);
#20447=PRODUCT_DEFINITION_FORMATION('',$,#20556);
#20448=PRODUCT_DEFINITION_FORMATION('',$,#20557);
#20449=PRODUCT_DEFINITION_FORMATION('',$,#20558);
#20450=PRODUCT_DEFINITION_FORMATION('',$,#20559);
#20451=PRODUCT_DEFINITION_FORMATION('',$,#20560);
#20452=PRODUCT_DEFINITION_FORMATION('',$,#20561);
#20453=PRODUCT_DEFINITION_FORMATION('',$,#20562);
#20454=PRODUCT_DEFINITION_FORMATION('',$,#20563);
#20455=PRODUCT_DEFINITION_FORMATION('',$,#20564);
#20456=PRODUCT_DEFINITION_FORMATION('',$,#20565);
#20457=PRODUCT_DEFINITION_FORMATION('',$,#20566);
#20458=PRODUCT_DEFINITION_FORMATION('',$,#20567);
#20459=PRODUCT_DEFINITION_FORMATION('',$,#20568);
#20460=PRODUCT_DEFINITION_FORMATION('',$,#20569);
#20461=PRODUCT_DEFINITION_FORMATION('',$,#20570);
#20462=PRODUCT_DEFINITION_FORMATION('',$,#20571);
#20463=PRODUCT_DEFINITION_FORMATION('',$,#20572);
#20464=PRODUCT_DEFINITION_FORMATION('',$,#20573);
#20465=PRODUCT_DEFINITION_FORMATION('',$,#20574);
#20466=PRODUCT_DEFINITION_FORMATION('',$,#20575);
#20467=PRODUCT_DEFINITION_FORMATION('',$,#20576);
#20468=PRODUCT_DEFINITION_FORMATION('',$,#20577);
#20469=PRODUCT_DEFINITION_FORMATION('',$,#20578);
#20470=PRODUCT_DEFINITION_FORMATION('',$,#20579);
#20471=PRODUCT_DEFINITION_FORMATION('',$,#20580);
#20472=PRODUCT_RELATED_PRODUCT_CATEGORY('PAT-013','PAT-013',(#20528));
#20473=PRODUCT_RELATED_PRODUCT_CATEGORY('Frame and belt envelope',
'Frame and belt envelope',(#20529));
#20474=PRODUCT_RELATED_PRODUCT_CATEGORY('Base','Base',(#20530));
#20475=PRODUCT_RELATED_PRODUCT_CATEGORY('Foot','Foot',(#20531));
#20476=PRODUCT_RELATED_PRODUCT_CATEGORY('Foot (1)','Foot (1)',(#20532));
#20477=PRODUCT_RELATED_PRODUCT_CATEGORY('Fixed bearing block',
'Fixed bearing block',(#20533));
#20478=PRODUCT_RELATED_PRODUCT_CATEGORY('Input outer spacer',
'Input outer spacer',(#20534));
#20479=PRODUCT_RELATED_PRODUCT_CATEGORY('Input bearing cap',
'Input bearing cap',(#20535));
#20480=PRODUCT_RELATED_PRODUCT_CATEGORY('Input bearing cap (1)',
'Input bearing cap (1)',(#20536));
#20481=PRODUCT_RELATED_PRODUCT_CATEGORY('Fixed bearing block (1)',
'Fixed bearing block (1)',(#20537));
#20482=PRODUCT_RELATED_PRODUCT_CATEGORY('Input outer spacer (1)',
'Input outer spacer (1)',(#20538));
#20483=PRODUCT_RELATED_PRODUCT_CATEGORY('Input bearing cap (2)',
'Input bearing cap (2)',(#20539));
#20484=PRODUCT_RELATED_PRODUCT_CATEGORY('Input bearing cap (3)',
'Input bearing cap (3)',(#20540));
#20485=PRODUCT_RELATED_PRODUCT_CATEGORY('Timing belt backing envelope',
'Timing belt backing envelope',(#20541));
#20486=PRODUCT_RELATED_PRODUCT_CATEGORY('Travel stop','Travel stop',(#20542));
#20487=PRODUCT_RELATED_PRODUCT_CATEGORY('Travel stop (1)',
'Travel stop (1)',(#20543));
#20488=PRODUCT_RELATED_PRODUCT_CATEGORY(
'Sealed Ball Bearing - 10 x 30 x 9 mm',
'Sealed Ball Bearing - 10 x 30 x 9 mm',(#20544));
#20489=PRODUCT_RELATED_PRODUCT_CATEGORY('Inner ring','Inner ring',(#20545));
#20490=PRODUCT_RELATED_PRODUCT_CATEGORY('Outer ring','Outer ring',(#20546));
#20491=PRODUCT_RELATED_PRODUCT_CATEGORY('Balls','Balls',(#20547));
#20492=PRODUCT_RELATED_PRODUCT_CATEGORY('Cage','Cage',(#20548));
#20493=PRODUCT_RELATED_PRODUCT_CATEGORY('Seals 2RS','Seals 2RS',(#20549));
#20494=PRODUCT_RELATED_PRODUCT_CATEGORY(
'Slotted Extrusion - 20 x 20 x 400 mm',
'Slotted Extrusion - 20 x 20 x 400 mm',(#20550));
#20495=PRODUCT_RELATED_PRODUCT_CATEGORY('Captive slot nut',
'Captive slot nut',(#20551));
#20496=PRODUCT_RELATED_PRODUCT_CATEGORY('M5x17.5 extrusion screw',
'M5x17.5 extrusion screw',(#20552));
#20497=PRODUCT_RELATED_PRODUCT_CATEGORY(
'Linear Guide Rail - 15 mm, 220 mm Long',
'Linear Guide Rail - 15 mm, 220 mm Long',(#20553));
#20498=PRODUCT_RELATED_PRODUCT_CATEGORY('Drive pulley and shaft',
'Drive pulley and shaft',(#20554));
#20499=PRODUCT_RELATED_PRODUCT_CATEGORY('Input shaft','Input shaft',(#20555));
#20500=PRODUCT_RELATED_PRODUCT_CATEGORY('Input inner spacer',
'Input inner spacer',(#20556));
#20501=PRODUCT_RELATED_PRODUCT_CATEGORY('Input inner sleeve',
'Input inner sleeve',(#20557));
#20502=PRODUCT_RELATED_PRODUCT_CATEGORY('Input M3 set screw',
'Input M3 set screw',(#20558));
#20503=PRODUCT_RELATED_PRODUCT_CATEGORY('Input M3 set screw (1)',
'Input M3 set screw (1)',(#20559));
#20504=PRODUCT_RELATED_PRODUCT_CATEGORY('Input end keeper',
'Input end keeper',(#20560));
#20505=PRODUCT_RELATED_PRODUCT_CATEGORY('Return pulley and shaft',
'Return pulley and shaft',(#20561));
#20506=PRODUCT_RELATED_PRODUCT_CATEGORY('Input shaft (1)',
'Input shaft (1)',(#20562));
#20507=PRODUCT_RELATED_PRODUCT_CATEGORY('Input inner spacer (1)',
'Input inner spacer (1)',(#20563));
#20508=PRODUCT_RELATED_PRODUCT_CATEGORY('Input inner sleeve (1)',
'Input inner sleeve (1)',(#20564));
#20509=PRODUCT_RELATED_PRODUCT_CATEGORY('Input M3 set screw (2)',
'Input M3 set screw (2)',(#20565));
#20510=PRODUCT_RELATED_PRODUCT_CATEGORY('Input M3 set screw (3)',
'Input M3 set screw (3)',(#20566));
#20511=PRODUCT_RELATED_PRODUCT_CATEGORY('Input end keeper (1)',
'Input end keeper (1)',(#20567));
#20512=PRODUCT_RELATED_PRODUCT_CATEGORY(
'Timing Pulley - 2 mm Pitch, 20 Teeth, 8 mm Bore',
'Timing Pulley - 2 mm Pitch, 20 Teeth, 8 mm Bore',(#20568));
#20513=PRODUCT_RELATED_PRODUCT_CATEGORY('Moving carriage',
'Moving carriage',(#20569));
#20514=PRODUCT_RELATED_PRODUCT_CATEGORY('Moving table','Moving table',(#20570));
#20515=PRODUCT_RELATED_PRODUCT_CATEGORY('Belt attachment bracket',
'Belt attachment bracket',(#20571));
#20516=PRODUCT_RELATED_PRODUCT_CATEGORY('Belt clamp jaw',
'Belt clamp jaw',(#20572));
#20517=PRODUCT_RELATED_PRODUCT_CATEGORY(
'Flanged Linear Guide Carriage - 15 mm',
'Flanged Linear Guide Carriage - 15 mm',(#20573));
#20518=PRODUCT_RELATED_PRODUCT_CATEGORY('Block','Block',(#20574));
#20519=PRODUCT_RELATED_PRODUCT_CATEGORY('End cap +','End cap +',(#20575));
#20520=PRODUCT_RELATED_PRODUCT_CATEGORY('End cap','End cap',(#20576));
#20521=PRODUCT_RELATED_PRODUCT_CATEGORY('Flat Washer - M5',
'Flat Washer - M5',(#20577));
#20522=PRODUCT_RELATED_PRODUCT_CATEGORY('Cap Screw - M5x20',
'Cap Screw - M5x20',(#20578));
#20523=PRODUCT_RELATED_PRODUCT_CATEGORY('M4x10 Cap Screw',
'M4x10 Cap Screw',(#20579));
#20524=PRODUCT_RELATED_PRODUCT_CATEGORY('Cap Screw - M4x16',
'Cap Screw - M4x16',(#20580));
#20525=APPLICATION_PROTOCOL_DEFINITION('international standard',
'automotive_design',2009,#20526);
#20526=APPLICATION_CONTEXT(
'Core Data for Automotive Mechanical Design Process');
#20527=PRODUCT_CONTEXT('part definition',#20526,'mechanical');
#20528=PRODUCT('PAT-013','PAT-013',
'PAT-013',(#20527));
#20529=PRODUCT('Frame and belt envelope','Frame and belt envelope',
'Frame and belt envelope',(#20527));
#20530=PRODUCT('Base','Base','Base',(#20527));
#20531=PRODUCT('Foot','Foot','Foot',(#20527));
#20532=PRODUCT('Foot (1)','Foot (1)','Foot (1)',(#20527));
#20533=PRODUCT('Fixed bearing block','Fixed bearing block',
'Fixed bearing block',(#20527));
#20534=PRODUCT('Input outer spacer','Input outer spacer',
'Input outer spacer',(#20527));
#20535=PRODUCT('Input bearing cap','Input bearing cap',
'Input bearing cap',(#20527));
#20536=PRODUCT('Input bearing cap (1)','Input bearing cap (1)',
'Input bearing cap (1)',(#20527));
#20537=PRODUCT('Fixed bearing block (1)','Fixed bearing block (1)',
'Fixed bearing block (1)',(#20527));
#20538=PRODUCT('Input outer spacer (1)','Input outer spacer (1)',
'Input outer spacer (1)',(#20527));
#20539=PRODUCT('Input bearing cap (2)','Input bearing cap (2)',
'Input bearing cap (2)',(#20527));
#20540=PRODUCT('Input bearing cap (3)','Input bearing cap (3)',
'Input bearing cap (3)',(#20527));
#20541=PRODUCT('Timing belt backing envelope',
'Timing belt backing envelope','Timing belt backing envelope',(#20527));
#20542=PRODUCT('Travel stop','Travel stop','Travel stop',(#20527));
#20543=PRODUCT('Travel stop (1)','Travel stop (1)','Travel stop (1)',(#20527));
#20544=PRODUCT('Sealed Ball Bearing - 10 x 30 x 9 mm',
'Sealed Ball Bearing - 10 x 30 x 9 mm',
'Sealed Ball Bearing - 10 x 30 x 9 mm',(#20527));
#20545=PRODUCT('Inner ring','Inner ring','Inner ring',(#20527));
#20546=PRODUCT('Outer ring','Outer ring','Outer ring',(#20527));
#20547=PRODUCT('Balls','Balls','Balls',(#20527));
#20548=PRODUCT('Cage','Cage','Cage',(#20527));
#20549=PRODUCT('Seals 2RS','Seals 2RS','Seals 2RS',(#20527));
#20550=PRODUCT('Slotted Extrusion - 20 x 20 x 400 mm',
'Slotted Extrusion - 20 x 20 x 400 mm',
'Slotted Extrusion - 20 x 20 x 400 mm',(#20527));
#20551=PRODUCT('Captive slot nut','Captive slot nut','Captive slot nut',
(#20527));
#20552=PRODUCT('M5x17.5 extrusion screw','M5x17.5 extrusion screw',
'M5x17.5 extrusion screw',(#20527));
#20553=PRODUCT('Linear Guide Rail - 15 mm, 220 mm Long',
'Linear Guide Rail - 15 mm, 220 mm Long',
'Linear Guide Rail - 15 mm, 220 mm Long',(#20527));
#20554=PRODUCT('Drive pulley and shaft','Drive pulley and shaft',
'Drive pulley and shaft',(#20527));
#20555=PRODUCT('Input shaft','Input shaft','Input shaft',(#20527));
#20556=PRODUCT('Input inner spacer','Input inner spacer',
'Input inner spacer',(#20527));
#20557=PRODUCT('Input inner sleeve','Input inner sleeve',
'Input inner sleeve',(#20527));
#20558=PRODUCT('Input M3 set screw','Input M3 set screw',
'Input M3 set screw',(#20527));
#20559=PRODUCT('Input M3 set screw (1)','Input M3 set screw (1)',
'Input M3 set screw (1)',(#20527));
#20560=PRODUCT('Input end keeper','Input end keeper','Input end keeper',
(#20527));
#20561=PRODUCT('Return pulley and shaft','Return pulley and shaft',
'Return pulley and shaft',(#20527));
#20562=PRODUCT('Input shaft (1)','Input shaft (1)','Input shaft (1)',(#20527));
#20563=PRODUCT('Input inner spacer (1)','Input inner spacer (1)',
'Input inner spacer (1)',(#20527));
#20564=PRODUCT('Input inner sleeve (1)','Input inner sleeve (1)',
'Input inner sleeve (1)',(#20527));
#20565=PRODUCT('Input M3 set screw (2)','Input M3 set screw (2)',
'Input M3 set screw (2)',(#20527));
#20566=PRODUCT('Input M3 set screw (3)','Input M3 set screw (3)',
'Input M3 set screw (3)',(#20527));
#20567=PRODUCT('Input end keeper (1)','Input end keeper (1)',
'Input end keeper (1)',(#20527));
#20568=PRODUCT('Timing Pulley - 2 mm Pitch, 20 Teeth, 8 mm Bore',
'Timing Pulley - 2 mm Pitch, 20 Teeth, 8 mm Bore',
'Timing Pulley - 2 mm Pitch, 20 Teeth, 8 mm Bore',(#20527));
#20569=PRODUCT('Moving carriage','Moving carriage','Moving carriage',(#20527));
#20570=PRODUCT('Moving table','Moving table','Moving table',(#20527));
#20571=PRODUCT('Belt attachment bracket','Belt attachment bracket',
'Belt attachment bracket',(#20527));
#20572=PRODUCT('Belt clamp jaw','Belt clamp jaw','Belt clamp jaw',(#20527));
#20573=PRODUCT('Flanged Linear Guide Carriage - 15 mm',
'Flanged Linear Guide Carriage - 15 mm',
'Flanged Linear Guide Carriage - 15 mm',(#20527));
#20574=PRODUCT('Block','Block','Block',(#20527));
#20575=PRODUCT('End cap +','End cap +','End cap +',(#20527));
#20576=PRODUCT('End cap','End cap','End cap',(#20527));
#20577=PRODUCT('Flat Washer - M5','Flat Washer - M5','Flat Washer - M5',
(#20527));
#20578=PRODUCT('Cap Screw - M5x20','Cap Screw - M5x20',
'Cap Screw - M5x20',(#20527));
#20579=PRODUCT('M4x10 Cap Screw','M4x10 Cap Screw','M4x10 Cap Screw',(#20527));
#20580=PRODUCT('Cap Screw - M4x16','Cap Screw - M4x16',
'Cap Screw - M4x16',(#20527));
#20581=PRESENTATION_STYLE_ASSIGNMENT((#20587));
#20582=PRESENTATION_STYLE_ASSIGNMENT((#20588));
#20583=PRESENTATION_STYLE_ASSIGNMENT((#20589));
#20584=PRESENTATION_STYLE_ASSIGNMENT((#20590));
#20585=PRESENTATION_STYLE_ASSIGNMENT((#20591));
#20586=PRESENTATION_STYLE_ASSIGNMENT((#20592));
#20587=SURFACE_STYLE_USAGE(.BOTH.,#20593);
#20588=SURFACE_STYLE_USAGE(.BOTH.,#20594);
#20589=SURFACE_STYLE_USAGE(.BOTH.,#20595);
#20590=SURFACE_STYLE_USAGE(.BOTH.,#20596);
#20591=SURFACE_STYLE_USAGE(.BOTH.,#20597);
#20592=SURFACE_STYLE_USAGE(.BOTH.,#20598);
#20593=SURFACE_SIDE_STYLE('',(#20599));
#20594=SURFACE_SIDE_STYLE('',(#20600));
#20595=SURFACE_SIDE_STYLE('',(#20601));
#20596=SURFACE_SIDE_STYLE('',(#20602));
#20597=SURFACE_SIDE_STYLE('',(#20603));
#20598=SURFACE_SIDE_STYLE('',(#20604));
#20599=SURFACE_STYLE_FILL_AREA(#20605);
#20600=SURFACE_STYLE_FILL_AREA(#20606);
#20601=SURFACE_STYLE_FILL_AREA(#20607);
#20602=SURFACE_STYLE_FILL_AREA(#20608);
#20603=SURFACE_STYLE_FILL_AREA(#20609);
#20604=SURFACE_STYLE_FILL_AREA(#20610);
#20605=FILL_AREA_STYLE('Steel - Satin',(#20611));
#20606=FILL_AREA_STYLE('CAD Library Painted - Deep blue',(#20612));
#20607=FILL_AREA_STYLE('CAD Library Painted - Steel gray',(#20613));
#20608=FILL_AREA_STYLE('CAD Library Painted - Engineering blue',(#20614));
#20609=FILL_AREA_STYLE('CAD Library Painted - Graphite',(#20615));
#20610=FILL_AREA_STYLE('CAD Library Painted - Light blue',(#20616));
#20611=FILL_AREA_STYLE_COLOUR('Steel - Satin',#20617);
#20612=FILL_AREA_STYLE_COLOUR('CAD Library Painted - Deep blue',#20618);
#20613=FILL_AREA_STYLE_COLOUR('CAD Library Painted - Steel gray',#20619);
#20614=FILL_AREA_STYLE_COLOUR('CAD Library Painted - Engineering blue',
#20620);
#20615=FILL_AREA_STYLE_COLOUR('CAD Library Painted - Graphite',#20621);
#20616=FILL_AREA_STYLE_COLOUR('CAD Library Painted - Light blue',#20622);
#20617=COLOUR_RGB('Steel - Satin',0.627450980392157,0.627450980392157,0.627450980392157);
#20618=COLOUR_RGB('CAD Library Painted - Deep blue',0.0784313725490196,
0.203921568627451,0.349019607843137);
#20619=COLOUR_RGB('CAD Library Painted - Steel gray',0.592156862745098,
0.631372549019608,0.67843137254902);
#20620=COLOUR_RGB('CAD Library Painted - Engineering blue',0.12156862745098,
0.356862745098039,0.6);
#20621=COLOUR_RGB('CAD Library Painted - Graphite',0.168627450980392,0.192156862745098,
0.231372549019608);
#20622=COLOUR_RGB('CAD Library Painted - Light blue',0.286274509803922,
0.552941176470588,0.780392156862745);
#20623=COLOUR_RGB('Dark Blue',0.08,0.2,0.34);
#20624=FILL_AREA_STYLE_COLOUR('',#20623);
#20625=FILL_AREA_STYLE('',(#20624));
#20626=SURFACE_STYLE_FILL_AREA(#20625);
#20627=SURFACE_SIDE_STYLE('',(#20626));
#20628=SURFACE_STYLE_USAGE(.BOTH.,#20627);
#20629=PRESENTATION_STYLE_ASSIGNMENT((#20628));
#20630=COLOUR_RGB('Light Blue',0.38,0.62,0.78);
#20631=FILL_AREA_STYLE_COLOUR('',#20630);
#20632=FILL_AREA_STYLE('',(#20631));
#20633=SURFACE_STYLE_FILL_AREA(#20632);
#20634=SURFACE_SIDE_STYLE('',(#20633));
#20635=SURFACE_STYLE_USAGE(.BOTH.,#20634);
#20636=PRESENTATION_STYLE_ASSIGNMENT((#20635));
#20637=COLOUR_RGB('Sky Blue',0.24,0.69,0.87);
#20638=FILL_AREA_STYLE_COLOUR('',#20637);
#20639=FILL_AREA_STYLE('',(#20638));
#20640=SURFACE_STYLE_FILL_AREA(#20639);
#20641=SURFACE_SIDE_STYLE('',(#20640));
#20642=SURFACE_STYLE_USAGE(.BOTH.,#20641);
#20643=PRESENTATION_STYLE_ASSIGNMENT((#20642));
#20644=COLOUR_RGB('Grey',0.48,0.52,0.57);
#20645=FILL_AREA_STYLE_COLOUR('',#20644);
#20646=FILL_AREA_STYLE('',(#20645));
#20647=SURFACE_STYLE_FILL_AREA(#20646);
#20648=SURFACE_SIDE_STYLE('',(#20647));
#20649=SURFACE_STYLE_USAGE(.BOTH.,#20648);
#20650=PRESENTATION_STYLE_ASSIGNMENT((#20649));
#20651=COLOUR_RGB('Black',0.12,0.14,0.17);
#20652=FILL_AREA_STYLE_COLOUR('',#20651);
#20653=FILL_AREA_STYLE('',(#20652));
#20654=SURFACE_STYLE_FILL_AREA(#20653);
#20655=SURFACE_SIDE_STYLE('',(#20654));
#20656=SURFACE_STYLE_USAGE(.BOTH.,#20655);
#20657=PRESENTATION_STYLE_ASSIGNMENT((#20656));
#20658=COLOUR_RGB('Off White',0.89,0.88,0.83);
#20659=FILL_AREA_STYLE_COLOUR('',#20658);
#20660=FILL_AREA_STYLE('',(#20659));
#20661=SURFACE_STYLE_FILL_AREA(#20660);
#20662=SURFACE_SIDE_STYLE('',(#20661));
#20663=SURFACE_STYLE_USAGE(.BOTH.,#20662);
#20664=PRESENTATION_STYLE_ASSIGNMENT((#20663));
ENDSEC;
END-ISO-10303-21;
